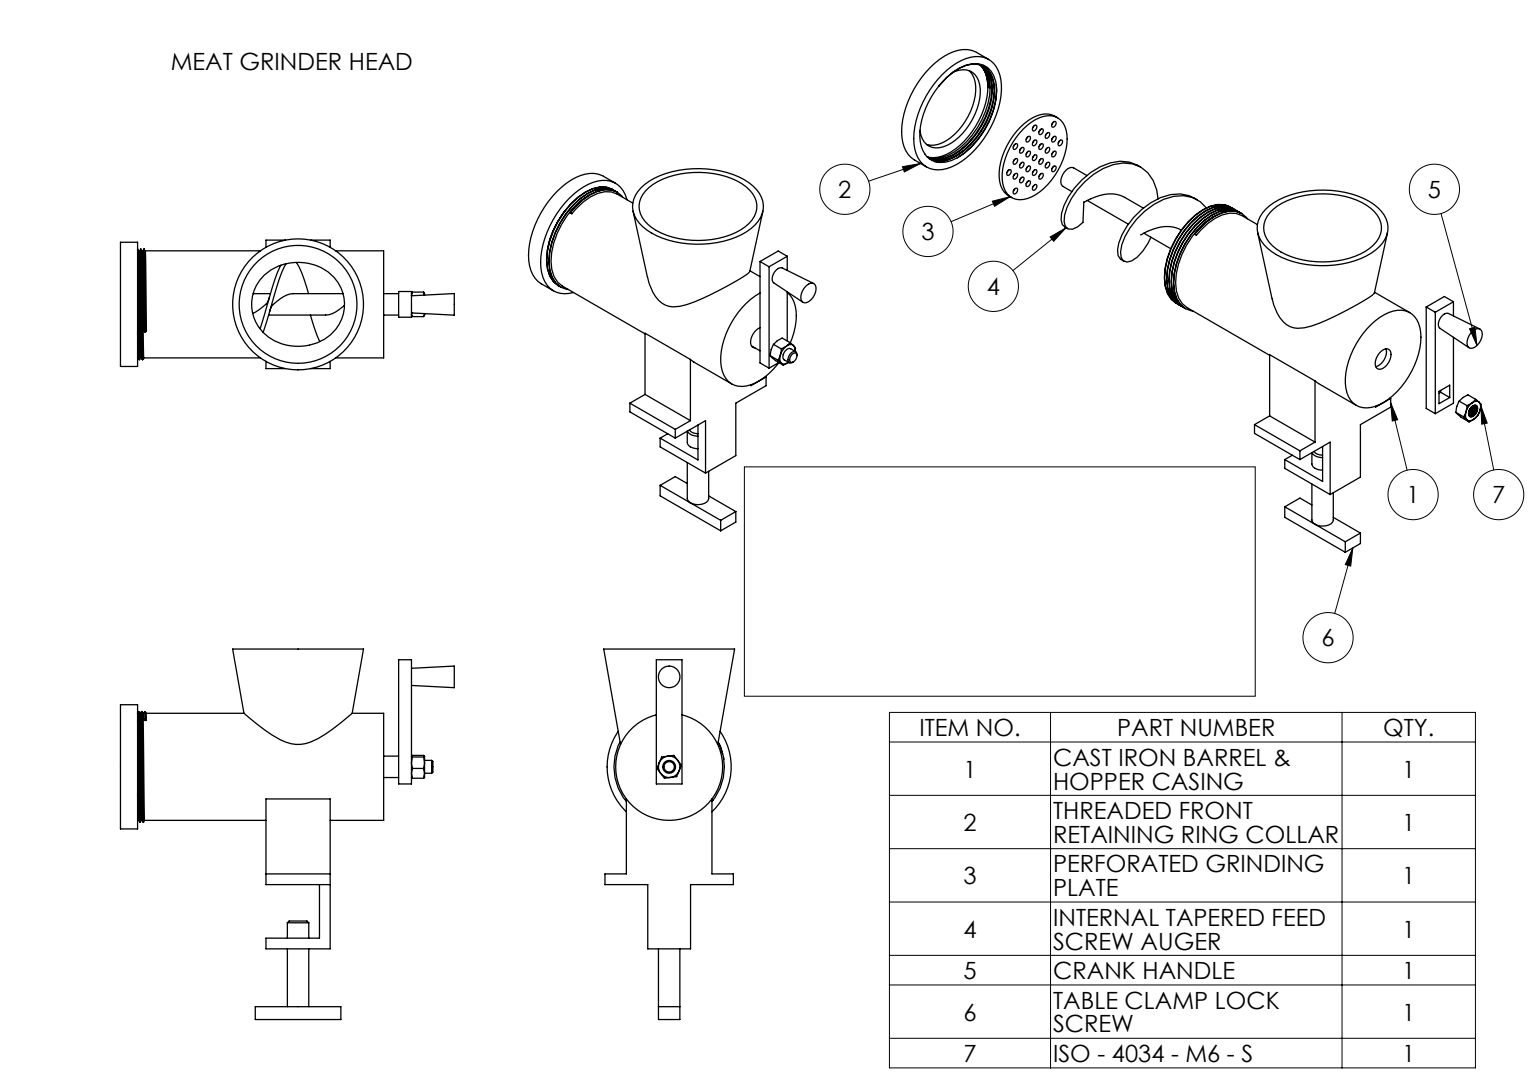
ISO-10303-21;
HEADER;
FILE_DESCRIPTION (('STEP AP214'),
    '1' );
FILE_NAME ('MAS-170',
    '2026-10-22T10:02:39',
    ( '' ),
    ( '' ),
    'SwSTEP 2.0',
    'SolidWorks 2026',
    '' );
FILE_SCHEMA (( 'AUTOMOTIVE_DESIGN' ));
ENDSEC;

DATA;
#1 = CARTESIAN_POINT ( 'NONE',  ( -15.00000000000000000, 55.00000000000000000, -20.00000000000000000 ) ) ;
#2 = AXIS2_PLACEMENT_3D ( 'NONE', #2206, #5818, #4912 ) ;
#3 = CARTESIAN_POINT ( 'NONE',  ( -24.57385867913225042, 55.01967498809302981, -0.01734603766092172178 ) ) ;
#4 = APPLICATION_PROTOCOL_DEFINITION ( 'draft international standard', 'automotive_design', 1998, #10813 ) ;
#5 = CARTESIAN_POINT ( 'NONE',  ( -21.63041020058595976, 76.92929161012460781, 1.799941901431467484 ) ) ;
#6 = VECTOR ( 'NONE', #483, 1000.000000000000000 ) ;
#7 = CIRCLE ( 'NONE', #1554, 1.500000000000001332 ) ;
#8 = CARTESIAN_POINT ( 'NONE',  ( -15.84874342590320673, 58.76832510134365606, 3.302529147201385129 ) ) ;
#9 = ORIENTED_EDGE ( 'NONE', *, *, #6036, .T. ) ;
#10 = CARTESIAN_POINT ( 'NONE',  ( -15.00000000000000000, 5.000000000000000000, 20.00000000000000000 ) ) ;
#11 = VERTEX_POINT ( 'NONE', #2092 ) ;
#12 = CARTESIAN_POINT ( 'NONE',  ( 7.477680471578420196, 36.66673471410030061, 10.56605622896702990 ) ) ;
#13 = CARTESIAN_POINT ( 'NONE',  ( -73.34375000204839523, 73.25176868561975141, -18.25176868561974430 ) ) ;
#14 = AXIS2_PLACEMENT_3D ( 'NONE', #9720, #5068, #10559 ) ;
#15 = EDGE_LOOP ( 'NONE', ( #10379, #7375, #3120, #371 ) ) ;
#16 = CARTESIAN_POINT ( 'NONE',  ( -75.12500000204838102, 44.30836144126050158, -25.81189881249999374 ) ) ;
#17 = CARTESIAN_POINT ( 'NONE',  ( 3.697305843545918513, 35.98616635274733255, -8.992456113074794644 ) ) ;
#18 = EDGE_CURVE ( 'NONE', #2366, #7152, #6007, .T. ) ;
#19 = VERTEX_POINT ( 'NONE', #7735 ) ;
#20 = APPLICATION_CONTEXT ( 'automotive_design' ) ;
#21 = CARTESIAN_POINT ( 'NONE',  ( -78.00000000000001421, 59.24264068711927678, 4.242644059037073312 ) ) ;
#22 = CARTESIAN_POINT ( 'NONE',  ( 18.90732451447525975, 55.01449046109523522, 0.007799356525960917524 ) ) ;
#23 = ORIENTED_EDGE ( 'NONE', *, *, #2675, .T. ) ;
#24 = CARTESIAN_POINT ( 'NONE',  ( -46.47759630686348942, 71.80626330759284315, -12.92347896748408509 ) ) ;
#25 = CARTESIAN_POINT ( 'NONE',  ( -13.52239577877046095, 75.98118489547775312, -2.745668029642679642 ) ) ;
#26 = CARTESIAN_POINT ( 'NONE',  ( 0.000000000000000000, 5.773502691896260863, -5.653418012614792154 ) ) ;
#27 = DIRECTION ( 'NONE',  ( 0.000000000000000000, 0.000000000000000000, 1.000000000000000000 ) ) ;
#28 = CARTESIAN_POINT ( 'NONE',  ( -78.00000000000001421, 50.75735931288069480, -11.22791868944003824 ) ) ;
#29 = DIRECTION ( 'NONE',  ( -1.000000000000000000, -0.000000000000000000, -0.000000000000000000 ) ) ;
#30 = VERTEX_POINT ( 'NONE', #8511 ) ;
#31 = CARTESIAN_POINT ( 'NONE',  ( -76.62500000409677625, 55.00000000000000000, 24.99999999999999645 ) ) ;
#32 = CARTESIAN_POINT ( 'NONE',  ( -54.99787500575298083, 55.00175321043320764, 0.0009066026748406779724 ) ) ;
#33 = CARTESIAN_POINT ( 'NONE',  ( -34.13164850161200548, 51.02358645912743640, -3.048757558511538068 ) ) ;
#34 = CARTESIAN_POINT ( 'NONE',  ( -80.00000000000001421, 63.48528137423857487, 8.485284746156350977 ) ) ;
#35 = EDGE_CURVE ( 'NONE', #6873, #1790, #10415, .T. ) ;
#36 = DIRECTION ( 'NONE',  ( 0.000000000000000000, 1.000000000000000000, 0.000000000000000000 ) ) ;
#37 = ORIENTED_EDGE ( 'NONE', *, *, #7774, .F. ) ;
#38 = CARTESIAN_POINT ( 'NONE',  ( -1.477628194636992243, 49.49121550494065502, -20.47411891050684218 ) ) ;
#39 = LINE ( 'NONE', #6477, #6145 ) ;
#40 = CARTESIAN_POINT ( 'NONE',  ( 10.96071222073927132, 53.39157304099641266, 4.745597011473480009 ) ) ;
#41 = CARTESIAN_POINT ( 'NONE',  ( -74.00000000204839523, 29.18810118750000981, 10.69163855873950020 ) ) ;
#42 = CARTESIAN_POINT ( 'NONE',  ( -78.87500000204838102, 65.69163855873949842, 25.81189881250000440 ) ) ;
#43 = VERTEX_POINT ( 'NONE', #10470 ) ;
#44 = CARTESIAN_POINT ( 'NONE',  ( -76.71875000204839523, 29.18810118750000271, 4.741568889096522788E-15 ) ) ;
#45 = ORIENTED_EDGE ( 'NONE', *, *, #4555, .T. ) ;
#46 = CARTESIAN_POINT ( 'NONE',  ( 3.204603673684104592, 51.02314964536983410, -3.048084100943247332 ) ) ;
#47 = CARTESIAN_POINT ( 'NONE',  ( -28.33520174651890144, 42.04728119469179148, 5.364820852706460030 ) ) ;
#48 = EDGE_CURVE ( 'NONE', #8851, #443, #4129, .T. ) ;
#49 = DIRECTION ( 'NONE',  ( 1.000000000000000000, 0.000000000000000000, 0.000000000000000000 ) ) ;
#50 = LINE ( 'NONE', #11190, #9309 ) ;
#51 = CARTESIAN_POINT ( 'NONE',  ( -78.03125000000002842, 79.99999999999992895, 10.35533905932734378 ) ) ;
#52 = VERTEX_POINT ( 'NONE', #2215 ) ;
#53 = CARTESIAN_POINT ( 'NONE',  ( -79.25000000000000000, 55.00000000000000000, 24.99999999999999645 ) ) ;
#54 = CARTESIAN_POINT ( 'NONE',  ( -72.59375000204838102, 55.00000000000000000, 25.81189881249999729 ) ) ;
#55 = EDGE_CURVE ( 'NONE', #2377, #9420, #11722, .T. ) ;
#56 = CARTESIAN_POINT ( 'NONE',  ( 0.000000000000000000, 0.000000000000000000, -6.099999999999999645 ) ) ;
#57 = B_SPLINE_CURVE_WITH_KNOTS ( 'NONE', 3,
 ( #11398, #9893, #5467, #4168 ),
 .UNSPECIFIED., .F., .F.,
 ( 4, 4 ),
 ( 2.380735200816727406E-07, 0.002921158011986720298 ),
 .UNSPECIFIED. ) ;
#58 = VECTOR ( 'NONE', #4245, 1000.000000000000000 ) ;
#59 = CARTESIAN_POINT ( 'NONE',  ( -47.09272475956910142, 55.02483394329467359, -0.008490977716145282211 ) ) ;
#60 = SHAPE_DEFINITION_REPRESENTATION ( #9305, #2176 ) ;
#61 = ADVANCED_FACE ( 'NONE', ( #1382, #293, #5043, #8690, #5765, #7618, #472, #11246, #4861, #6728, #10360, #351, #7675, #5881, #9524, #9811, #11776, #5272, #7139, #8090, #4373, #7912, #9698, #7079, #1495, #5216, #7192, #9040, #7965, #8982 ), #11541, .F. ) ;
#62 = CARTESIAN_POINT ( 'NONE',  ( -19.12261397941723473, 74.85860496676178855, 9.489298872914485372 ) ) ;
#63 = ADVANCED_FACE ( 'NONE', ( #6296 ), #11663, .F. ) ;
#64 = EDGE_CURVE ( 'NONE', #4200, #8679, #1605, .T. ) ;
#65 = DIRECTION ( 'NONE',  ( -0.000000000000000000, -1.000000000000000000, -0.000000000000000000 ) ) ;
#66 = VERTEX_POINT ( 'NONE', #6237 ) ;
#67 = DIRECTION ( 'NONE',  ( -1.000000000000000000, 0.000000000000000000, 0.000000000000000000 ) ) ;
#68 = FACE_OUTER_BOUND ( 'NONE', #814, .T. ) ;
#69 = VERTEX_POINT ( 'NONE', #11601 ) ;
#70 = CARTESIAN_POINT ( 'NONE',  ( -62.96917444215183224, 46.00616310598284286, 19.01165851688606523 ) ) ;
#71 = CARTESIAN_POINT ( 'NONE',  ( -71.59560441781462714, 80.81189881250000440, 6.916273779317701376 ) ) ;
#72 = EDGE_CURVE ( 'NONE', #8769, #5516, #701, .T. ) ;
#73 = ADVANCED_FACE ( 'NONE', ( #817 ), #4433, .F. ) ;
#74 = ORIENTED_EDGE ( 'NONE', *, *, #10875, .F. ) ;
#75 = EDGE_CURVE ( 'NONE', #3733, #9858, #3524, .T. ) ;
#76 = CARTESIAN_POINT ( 'NONE',  ( -72.50000000204839523, 29.18810118750000981, 10.69163855873950020 ) ) ;
#77 = CARTESIAN_POINT ( 'NONE',  ( -27.49360061100878738, 37.45598436699922473, 11.71495266747331421 ) ) ;
#78 = DIRECTION ( 'NONE',  ( -1.000000000000000000, 0.000000000000000000, 0.000000000000000000 ) ) ;
#79 = EDGE_LOOP ( 'NONE', ( #6944, #10404, #6581, #2124 ) ) ;
#80 = CARTESIAN_POINT ( 'NONE',  ( -12.37832547621337476, 59.49517489534859749, -2.213937092042313814 ) ) ;
#81 = COLOUR_RGB ( '',0.8941176470588234615, 0.8941176470588234615, 0.8941176470588234615 ) ;
#82 = CARTESIAN_POINT ( 'NONE',  ( -3.477628190354089099, 49.49309465598528845, -20.46958112014059950 ) ) ;
#83 = ORIENTED_EDGE ( 'NONE', *, *, #6664, .F. ) ;
#84 = CARTESIAN_POINT ( 'NONE',  ( -23.14426256960421924, 52.25445662165124361, 21.02210202263520600 ) ) ;
#85 = CARTESIAN_POINT ( 'NONE',  ( -68.81799204399976588, 34.52608862562686909, 5.501299279293338174 ) ) ;
#86 = LINE ( 'NONE', #1108, #4140 ) ;
#87 = DIRECTION ( 'NONE',  ( 1.000000000000000000, 0.000000000000000000, 0.000000000000000000 ) ) ;
#88 = LINE ( 'NONE', #7135, #10139 ) ;
#89 = VERTEX_POINT ( 'NONE', #9752 ) ;
#90 = CARTESIAN_POINT ( 'NONE',  ( -78.00000000000002842, 54.99999999999998579, 15.47056612039490986 ) ) ;
#91 = CARTESIAN_POINT ( 'NONE',  ( -44.20488284339200646, 55.00025175640378450, -0.002624240123811788852 ) ) ;
#92 = CARTESIAN_POINT ( 'NONE',  ( -56.68145153021548310, 56.29769244905448744, 4.839614506206188160 ) ) ;
#93 = CARTESIAN_POINT ( 'NONE',  ( 9.999999999999994671, -24.99999999999999645, 10.00000000000000000 ) ) ;
#94 = CARTESIAN_POINT ( 'NONE',  ( 47.00000000000000000, 55.00000000000000000, 0.000000000000000000 ) ) ;
#95 = CARTESIAN_POINT ( 'NONE',  ( -6.249156589778054105, 55.68730665650835476, -7.012895309292545676 ) ) ;
#96 = VERTEX_POINT ( 'NONE', #6118 ) ;
#97 = DIRECTION ( 'NONE',  ( 0.000000000000000000, -0.000000000000000000, 1.000000000000000000 ) ) ;
#98 = CARTESIAN_POINT ( 'NONE',  ( -71.75000000204838102, 80.81189881250000440, -10.69163855873948954 ) ) ;
#99 = CARTESIAN_POINT ( 'NONE',  ( 3.371861548457865722E-15, 110.0000000000000000, -27.53333900685068869 ) ) ;
#100 = CARTESIAN_POINT ( 'NONE',  ( -3.000000000000000000, 0.000000000000000000, -1.753742857142857048 ) ) ;
#101 = CARTESIAN_POINT ( 'NONE',  ( 0.000000000000000000, -24.99999999999999645, -5.000000000000000000 ) ) ;
#102 = CARTESIAN_POINT ( 'NONE',  ( -80.00000000000002842, 38.02943725152282184, 3.371917797929946392E-06 ) ) ;
#103 = AXIS2_PLACEMENT_3D ( 'NONE', #3802, #8297, #78 ) ;
#104 = ORIENTED_EDGE ( 'NONE', *, *, #11406, .F. ) ;
#105 = CARTESIAN_POINT ( 'NONE',  ( -77.65625000204839523, 73.25176868561975141, -18.25176868561974430 ) ) ;
#106 = ORIENTED_EDGE ( 'NONE', *, *, #10406, .T. ) ;
#107 = CARTESIAN_POINT ( 'NONE',  ( 24.10175047695886619, 78.98596163070220655, -7.059706225875322261 ) ) ;
#108 = CARTESIAN_POINT ( 'NONE',  ( -34.53957387867419015, 43.82314937793580611, -8.587433708483555250 ) ) ;
#109 = VECTOR ( 'NONE', #311, 1000.000000000000000 ) ;
#110 = CARTESIAN_POINT ( 'NONE',  ( -77.75000000204839523, 65.69163855873948421, -25.81189881250000084 ) ) ;
#111 = EDGE_CURVE ( 'NONE', #9073, #8979, #3345, .T. ) ;
#112 = DIRECTION ( 'NONE',  ( 0.000000000000000000, -0.000000000000000000, 1.000000000000000000 ) ) ;
#113 = DIRECTION ( 'NONE',  ( 0.000000000000000000, 0.000000000000000000, 1.000000000000000000 ) ) ;
#114 = ORIENTED_EDGE ( 'NONE', *, *, #10655, .T. ) ;
#115 = VECTOR ( 'NONE', #7085, 1000.000000000000000 ) ;
#116 = CARTESIAN_POINT ( 'NONE',  ( -78.31250000000000000, 72.67766952966368876, -17.67766952966368876 ) ) ;
#117 = CARTESIAN_POINT ( 'NONE',  ( -78.50000000409677625, 80.00000000000000000, -1.530808498934191324E-15 ) ) ;
#118 = CIRCLE ( 'NONE', #8173, 1.500000000000001332 ) ;
#119 = CARTESIAN_POINT ( 'NONE',  ( -78.00000000000001421, 50.75735931288069480, -12.72791868944003824 ) ) ;
#120 = DIRECTION ( 'NONE',  ( 1.000000000000000000, 0.000000000000000000, -0.000000000000000000 ) ) ;
#121 = CARTESIAN_POINT ( 'NONE',  ( -53.33538954556567546, 54.99810722428492937, -0.002143453996954131253 ) ) ;
#122 = SHAPE_DEFINITION_REPRESENTATION ( #1837, #423 ) ;
#123 = B_SPLINE_CURVE_WITH_KNOTS ( 'NONE', 3,
 ( #9839, #9954, #7047, #10669, #4339, #2656 ),
 .UNSPECIFIED., .F., .F.,
 ( 4, 2, 4 ),
 ( 0.008070708573309213693, 0.009531758523483282314, 0.01099280847365734920 ),
 .UNSPECIFIED. ) ;
#124 = CARTESIAN_POINT ( 'NONE',  ( -10.64432325360710152, 68.67941443230903076, -17.23560473394323367 ) ) ;
#125 = AXIS2_PLACEMENT_3D ( 'NONE', #5377, #67, #9915 ) ;
#126 = CARTESIAN_POINT ( 'NONE',  ( -5.000000000000000000, 0.000000000000000000, -6.099999999999999645 ) ) ;
#127 = AXIS2_PLACEMENT_3D ( 'NONE', #5632, #97, #11119 ) ;
#128 = ORIENTED_EDGE ( 'NONE', *, *, #8290, .T. ) ;
#129 = CARTESIAN_POINT ( 'NONE',  ( -79.34375000000000000, 65.35533905932734910, 24.99999999999997158 ) ) ;
#130 = CYLINDRICAL_SURFACE ( 'NONE', #5375, 1.500000000000000000 ) ;
#131 = VERTEX_POINT ( 'NONE', #8809 ) ;
#132 = CARTESIAN_POINT ( 'NONE',  ( -6.160267096003628318, 59.12214581854949103, -20.69010011304746044 ) ) ;
#133 = PRODUCT_DEFINITION ( 'UNKNOWN', '', #852, #2465 ) ;
#134 = CARTESIAN_POINT ( 'NONE',  ( -76.71875000204839523, 29.18810118750000271, 4.741568889096522788E-15 ) ) ;
#135 = CARTESIAN_POINT ( 'NONE',  ( -15.00000000000000355, 5.000000000000000000, -29.99999999999999289 ) ) ;
#136 = CARTESIAN_POINT ( 'NONE',  ( -6.214759040711413718, 65.81103152010582846, -18.03762937187994453 ) ) ;
#137 = CARTESIAN_POINT ( 'NONE',  ( -46.52239103091250172, 73.32882989972571863, -10.56393531560676102 ) ) ;
#138 = ORIENTED_EDGE ( 'NONE', *, *, #9495, .F. ) ;
#139 = LINE ( 'NONE', #1945, #11400 ) ;
#140 = EDGE_CURVE ( 'NONE', #7402, #8679, #2318, .T. ) ;
#141 = CARTESIAN_POINT ( 'NONE',  ( 46.99999999999999289, 58.53553390593273065, 3.535533905932731091 ) ) ;
#142 = CARTESIAN_POINT ( 'NONE',  ( 4.636023424558444184, 34.00634798409771520, 1.031279783234476222 ) ) ;
#143 = VECTOR ( 'NONE', #3904, 1000.000000000000000 ) ;
#144 = ORIENTED_EDGE ( 'NONE', *, *, #11561, .T. ) ;
#145 = CARTESIAN_POINT ( 'NONE',  ( -34.81092923608149192, 36.62878417468885317, -10.58136149031614970 ) ) ;
#146 = CARTESIAN_POINT ( 'NONE',  ( -70.34104699118840642, 33.99562393659799397, 0.006612473344882377653 ) ) ;
#147 = CARTESIAN_POINT ( 'NONE',  ( -73.34375000409679046, 30.00000000000001421, 10.35533905932739174 ) ) ;
#148 = DIRECTION ( 'NONE',  ( -1.000000000000000000, -0.000000000000000000, -0.000000000000000000 ) ) ;
#149 = EDGE_CURVE ( 'NONE', #1776, #658, #10646, .T. ) ;
#150 = CYLINDRICAL_SURFACE ( 'NONE', #7865, 1.499999999999999556 ) ;
#151 = EDGE_CURVE ( 'NONE', #658, #760, #3805, .T. ) ;
#152 = ORIENTED_EDGE ( 'NONE', *, *, #4340, .T. ) ;
#153 = DIRECTION ( 'NONE',  ( 0.000000000000000000, -0.000000000000000000, 1.000000000000000000 ) ) ;
#154 = CARTESIAN_POINT ( 'NONE',  ( -35.76380172564871884, 55.01086174631173975, 0.005834152228799136322 ) ) ;
#155 = CARTESIAN_POINT ( 'NONE',  ( -44.62221111874860213, 58.76649436596603948, -3.304682393689729381 ) ) ;
#156 = DIRECTION ( 'NONE',  ( -0.000000000000000000, -1.000000000000000000, -0.000000000000000000 ) ) ;
#157 = FACE_OUTER_BOUND ( 'NONE', #10390, .T. ) ;
#158 = CARTESIAN_POINT ( 'NONE',  ( -6.833556764572190190, 56.37289815856257746, -6.894355924324841567 ) ) ;
#159 = AXIS2_PLACEMENT_3D ( 'NONE', #745, #8186, #2789 ) ;
#160 = ORIENTED_EDGE ( 'NONE', *, *, #1242, .F. ) ;
#161 = CARTESIAN_POINT ( 'NONE',  ( 9.477680475861957277, 36.67126955513442255, 10.56417786655960356 ) ) ;
#162 = CARTESIAN_POINT ( 'NONE',  ( 0.000000000000000000, 0.000000000000000000, -0.01270000000000047133 ) ) ;
#163 = LINE ( 'NONE', #11122, #11282 ) ;
#164 = FACE_BOUND ( 'NONE', #3650, .T. ) ;
#165 = CARTESIAN_POINT ( 'NONE',  ( -12.37866201454132487, 69.98577131611273217, -20.01755997183146718 ) ) ;
#166 = CARTESIAN_POINT ( 'NONE',  ( -74.56250000204839523, 80.81189881250001861, 10.69163855873948599 ) ) ;
#167 = ORIENTED_EDGE ( 'NONE', *, *, #2613, .F. ) ;
#168 = CARTESIAN_POINT ( 'NONE',  ( -78.59375000204839523, 55.00000000000000000, 25.81189881249999729 ) ) ;
#169 = CIRCLE ( 'NONE', #3240, 1.500000000000001332 ) ;
#170 = ORIENTED_EDGE ( 'NONE', *, *, #3166, .T. ) ;
#171 = CARTESIAN_POINT ( 'NONE',  ( 3.392634454741613848, 65.79950035100726780, -22.54765914078175015 ) ) ;
#172 = AXIS2_PLACEMENT_3D ( 'NONE', #8865, #9866, #7078 ) ;
#173 = CARTESIAN_POINT ( 'NONE',  ( -30.96365390035560239, 40.99197526476194042, -0.6880654886566857087 ) ) ;
#174 = FACE_OUTER_BOUND ( 'NONE', #11292, .T. ) ;
#175 = ADVANCED_FACE ( 'NONE', ( #10161 ), #9210, .T. ) ;
#176 =( BOUNDED_CURVE ( )  B_SPLINE_CURVE ( 2, ( #5683, #4899, #11229, #6928, #8370, #6645, #9381, #4776, #5808 ),
 .UNSPECIFIED., .F., .T. ) 
 B_SPLINE_CURVE_WITH_KNOTS ( ( 3, 2, 2, 2, 3 ),
 ( 0.3333333333333335924, 0.3541666666666669627, 0.3750000000000003331, 0.3958333333333336479, 0.4166666666666670182 ),
 .UNSPECIFIED. ) 
 CURVE ( )  GEOMETRIC_REPRESENTATION_ITEM ( )  RATIONAL_B_SPLINE_CURVE ( ( 0.9999999999999990008, 0.9238795325112877377, 1.000000000000000000, 0.9238795325112867385, 1.000000000000000000, 0.9238795325112867385, 1.000000000000000000, 0.9238795325112855172, 1.000000000000001110 ) ) 
 REPRESENTATION_ITEM ( '' )  );
#177 = CARTESIAN_POINT ( 'NONE',  ( -75.00000000000000000, 63.49954157109033304, -24.30489545910771909 ) ) ;
#178 = CARTESIAN_POINT ( 'NONE',  ( -15.00000000000000355, 0.000000000000000000, -29.99999999999999289 ) ) ;
#179 = VECTOR ( 'NONE', #1295, 1000.000000000000000 ) ;
#180 = CIRCLE ( 'NONE', #6902, 2.500000000000000000 ) ;
#181 = EDGE_LOOP ( 'NONE', ( #6646, #3991, #9037, #3173 ) ) ;
#182 = FACE_OUTER_BOUND ( 'NONE', #3755, .T. ) ;
#183 = CYLINDRICAL_SURFACE ( 'NONE', #11845, 1.500000000000000444 ) ;
#184 = DIRECTION ( 'NONE',  ( 0.000000000000000000, 0.000000000000000000, 1.000000000000000000 ) ) ;
#185 = CARTESIAN_POINT ( 'NONE',  ( 0.000000000000000000, 0.000000000000000000, -2.617914285714285416 ) ) ;
#186 = CARTESIAN_POINT ( 'NONE',  ( 6.125158419864718873, 48.06305152834397632, -1.028633690847041704 ) ) ;
#187 = CARTESIAN_POINT ( 'NONE',  ( -7.638500494831339971, 67.00046308197731548, 18.44294210305378456 ) ) ;
#188 = DIRECTION ( 'NONE',  ( 0.000000000000000000, 0.000000000000000000, 1.000000000000000000 ) ) ;
#189 = EDGE_LOOP ( 'NONE', ( #2988, #1101, #3191 ) ) ;
#190 = EDGE_CURVE ( 'NONE', #2213, #10233, #9603, .T. ) ;
#191 = FACE_OUTER_BOUND ( 'NONE', #2836, .T. ) ;
#192 = DIRECTION ( 'NONE',  ( 0.000000000000000000, 0.000000000000000000, 1.000000000000000000 ) ) ;
#193 = VERTEX_POINT ( 'NONE', #2983 ) ;
#194 = CARTESIAN_POINT ( 'NONE',  ( -66.50782127702024127, 36.67013743889115318, 10.55179617378401247 ) ) ;
#195 = VECTOR ( 'NONE', #5572, 1000.000000000000000 ) ;
#196 = CARTESIAN_POINT ( 'NONE',  ( -78.68750000204839523, 65.69163855873949842, 25.81189881250000440 ) ) ;
#197 = EDGE_CURVE ( 'NONE', #1911, #3047, #4966, .T. ) ;
#198 = DIRECTION ( 'NONE',  ( 6.033820786006286457E-17, -1.000000000000000000, 0.000000000000000000 ) ) ;
#199 = CARTESIAN_POINT ( 'NONE',  ( -42.66281101964754896, 63.04450918361814615, -19.42252581123130639 ) ) ;
#200 = AXIS2_PLACEMENT_3D ( 'NONE', #7923, #603, #5167 ) ;
#201 = CONICAL_SURFACE ( 'NONE', #2897, 2.500000000000000000, 0.9599310885968755924 ) ;
#202 = PRESENTATION_STYLE_ASSIGNMENT (( #2843 ) ) ;
#203 = CARTESIAN_POINT ( 'NONE',  ( -30.99614452189004155, 33.97742542711323921, 0.0005215828242728561687 ) ) ;
#204 = ORIENTED_EDGE ( 'NONE', *, *, #9495, .T. ) ;
#205 = CARTESIAN_POINT ( 'NONE',  ( -71.93750000204838102, 44.30836144126049447, -25.81189881249999019 ) ) ;
#206 = EDGE_CURVE ( 'NONE', #6519, #11654, #6983, .T. ) ;
#207 = DIRECTION ( 'NONE',  ( -1.000000000000000000, -0.000000000000000000, -0.000000000000000000 ) ) ;
#208 = FACE_OUTER_BOUND ( 'NONE', #5773, .T. ) ;
#209 = ORIENTED_EDGE ( 'NONE', *, *, #10668, .T. ) ;
#210 = CARTESIAN_POINT ( 'NONE',  ( -56.17294560383920299, 66.73154858138525469, 17.54339796666672058 ) ) ;
#211 = CIRCLE ( 'NONE', #6745, 2.500000000000000000 ) ;
#212 = CARTESIAN_POINT ( 'NONE',  ( -61.00490302436042356, 55.00059028654953153, 21.02810969917934614 ) ) ;
#213 = FILL_AREA_STYLE_COLOUR ( '', #499 ) ;
#214 = CARTESIAN_POINT ( 'NONE',  ( -75.87500000409677625, 55.00000000000000000, -24.99999999999999645 ) ) ;
#215 = VECTOR ( 'NONE', #1197, 1000.000000000000000 ) ;
#216 = CARTESIAN_POINT ( 'NONE',  ( 53.00000000000000000, 51.46446609406726935, -3.535533905932738197 ) ) ;
#217 = CARTESIAN_POINT ( 'NONE',  ( 47.00000000000000000, 55.00000000000000000, 6.000000000000000000 ) ) ;
#218 = ORIENTED_EDGE ( 'NONE', *, *, #5065, .F. ) ;
#219 = CARTESIAN_POINT ( 'NONE',  ( -78.31250000000000000, 72.67766952966368876, -17.67766952966368876 ) ) ;
#220 = CARTESIAN_POINT ( 'NONE',  ( -14.57393009465980604, 54.98364064865898371, -0.001646604999752838971 ) ) ;
#221 = DIRECTION ( 'NONE',  ( 0.5000000000000005551, -0.8660254037844383745, 0.000000000000000000 ) ) ;
#222 = AXIS2_PLACEMENT_3D ( 'NONE', #671, #2237, #9611 ) ;
#223 = DIRECTION ( 'NONE',  ( -1.000000000000000000, -6.033820786006286457E-17, 0.000000000000000000 ) ) ;
#224 = CARTESIAN_POINT ( 'NONE',  ( 0.1668379413723253268, 49.14794564670181387, -3.906842406148068214 ) ) ;
#225 = ORIENTED_EDGE ( 'NONE', *, *, #438, .T. ) ;
#226 = CARTESIAN_POINT ( 'NONE',  ( 14.14423903981857755, 49.50929293985068114, 20.43023407247793699 ) ) ;
#227 = DIRECTION ( 'NONE',  ( 0.000000000000000000, 0.000000000000000000, 1.000000000000000000 ) ) ;
#228 = PLANE ( 'NONE',  #2565 ) ;
#229 = CARTESIAN_POINT ( 'NONE',  ( 73.00000000000000000, 91.95184441433917755, -3.614966813601447167E-16 ) ) ;
#230 = CARTESIAN_POINT ( 'NONE',  ( -71.84375000204838102, 73.25176868561975141, -18.25176868561974430 ) ) ;
#231 = CARTESIAN_POINT ( 'NONE',  ( -71.59560441781462714, 80.81189881250000440, 6.916273779317701376 ) ) ;
#232 = ORIENTED_EDGE ( 'NONE', *, *, #8402, .T. ) ;
#233 = CARTESIAN_POINT ( 'NONE',  ( -76.06250000409679046, 37.32233047033631124, -17.67766952966368166 ) ) ;
#234 = ORIENTED_EDGE ( 'NONE', *, *, #5652, .T. ) ;
#235 = CARTESIAN_POINT ( 'NONE',  ( 23.67201755683229081, 78.62200754200915753, -8.225812365109568702 ) ) ;
#236 = EDGE_CURVE ( 'NONE', #9206, #11519, #5249, .T. ) ;
#237 = CARTESIAN_POINT ( 'NONE',  ( -55.16972311799333539, 62.82217562642412645, 11.69677751401117405 ) ) ;
#238 = CARTESIAN_POINT ( 'NONE',  ( -78.87500000204839523, 65.69163855873949842, 25.81189881250000084 ) ) ;
#239 = CARTESIAN_POINT ( 'NONE',  ( -75.00000000000002842, 78.51577914341699227, 8.706246595591601078 ) ) ;
#240 = CARTESIAN_POINT ( 'NONE',  ( -2.500000000000000000, 3.061616997868383141E-16, -6.099999999999999645 ) ) ;
#241 = VERTEX_POINT ( 'NONE', #2085 ) ;
#242 = DIRECTION ( 'NONE',  ( 0.000000000000000000, -0.000000000000000000, 1.000000000000000000 ) ) ;
#243 = FACE_OUTER_BOUND ( 'NONE', #10356, .T. ) ;
#244 = LINE ( 'NONE', #4871, #4047 ) ;
#245 = FACE_BOUND ( 'NONE', #9079, .T. ) ;
#246 = CARTESIAN_POINT ( 'NONE',  ( -18.95794697780666027, 57.36371471763808927, 6.606639808170175598 ) ) ;
#247 = DIRECTION ( 'NONE',  ( -1.000000000000000000, -0.000000000000000000, -0.000000000000000000 ) ) ;
#248 = DIRECTION ( 'NONE',  ( -1.000000000000000000, -0.000000000000000000, -0.000000000000000000 ) ) ;
#249 = EDGE_LOOP ( 'NONE', ( #1338, #6982, #2879, #8696 ) ) ;
#250 = CARTESIAN_POINT ( 'NONE',  ( -78.00000000000002842, 42.27207793864211283, -4.242637315201479353 ) ) ;
#251 = CARTESIAN_POINT ( 'NONE',  ( 52.99999999999999289, 58.53553390593273065, 3.535533905932731091 ) ) ;
#252 = ORIENTED_EDGE ( 'NONE', *, *, #5075, .F. ) ;
#253 = CARTESIAN_POINT ( 'NONE',  ( -59.27472368810988002, 61.13901599248961105, 20.20251803659174783 ) ) ;
#254 = CARTESIAN_POINT ( 'NONE',  ( -75.87500000204839523, 80.81189881250001861, 10.69163855873948599 ) ) ;
#255 = DIRECTION ( 'NONE',  ( -1.000000000000000000, -0.000000000000000000, -0.000000000000000000 ) ) ;
#256 = CARTESIAN_POINT ( 'NONE',  ( -50.82691677660828589, 75.68920158268997511, 4.121780573430135597 ) ) ;
#257 =( NAMED_UNIT ( * ) SI_UNIT ( $, .STERADIAN. ) SOLID_ANGLE_UNIT ( ) );
#258 = DIRECTION ( 'NONE',  ( 0.000000000000000000, 1.000000000000000000, 0.000000000000000000 ) ) ;
#259 = ORIENTED_EDGE ( 'NONE', *, *, #6814, .T. ) ;
#260 = CIRCLE ( 'NONE', #1600, 3.000000000000000888 ) ;
#261 = CARTESIAN_POINT ( 'NONE',  ( -73.71875000204839523, 29.18810118750000271, 4.741568889096522788E-15 ) ) ;
#262 = PLANE ( 'NONE',  #3428 ) ;
#263 = ADVANCED_FACE ( 'NONE', ( #10291 ), #10352, .F. ) ;
#264 = CARTESIAN_POINT ( 'NONE',  ( -3.000000000000000000, 0.000000000000000000, -5.210428571428570521 ) ) ;
#265 = ORIENTED_EDGE ( 'NONE', *, *, #8549, .F. ) ;
#266 = ADVANCED_FACE ( 'NONE', ( #3949 ), #228, .F. ) ;
#267 = CARTESIAN_POINT ( 'NONE',  ( -58.49417186384191325, 59.10997037288393585, 20.69225924102262226 ) ) ;
#268 = CARTESIAN_POINT ( 'NONE',  ( 14.87282114002693234, 58.67269055319452065, 13.65170787854068024 ) ) ;
#269 = CYLINDRICAL_SURFACE ( 'NONE', #2101, 1.499999999999999556 ) ;
#270 = CARTESIAN_POINT ( 'NONE',  ( -76.34375000409679046, 30.00000000000001421, 10.35533905932739174 ) ) ;
#271 = FACE_OUTER_BOUND ( 'NONE', #5676, .T. ) ;
#272 = CARTESIAN_POINT ( 'NONE',  ( -72.06435441788595142, 79.99999999999991473, 6.698726029249561620 ) ) ;
#273 = ADVANCED_FACE ( 'NONE', ( #4913 ), #344, .F. ) ;
#274 = ORIENTED_EDGE ( 'NONE', *, *, #7349, .T. ) ;
#275 = CARTESIAN_POINT ( 'NONE',  ( -79.53125000000000000, 80.00000000000001421, 10.35533905932737397 ) ) ;
#276 = CARTESIAN_POINT ( 'NONE',  ( -68.24753854205350478, 55.02494518472502705, -0.0008082322394851507684 ) ) ;
#277 = AXIS2_PLACEMENT_3D ( 'NONE', #2600, #1465, #2419 ) ;
#278 = PLANE ( 'NONE',  #4388 ) ;
#279 = CARTESIAN_POINT ( 'NONE',  ( -15.00000000000000000, -24.99999999999999645, 10.00000000000000000 ) ) ;
#280 = CARTESIAN_POINT ( 'NONE',  ( -69.87738456456679614, 41.01771127808763140, 1.829669757797043994 ) ) ;
#281 = ORIENTED_EDGE ( 'NONE', *, *, #2765, .F. ) ;
#282 = DIRECTION ( 'NONE',  ( -1.000000000000000000, -0.000000000000000000, -0.000000000000000000 ) ) ;
#283 = CARTESIAN_POINT ( 'NONE',  ( 36.99999999999999289, 59.99999999999998579, 0.000000000000000000 ) ) ;
#284 = CARTESIAN_POINT ( 'NONE',  ( 53.00000000000000000, 51.46446609406726935, -3.535533905932738197 ) ) ;
#285 = DIRECTION ( 'NONE',  ( -0.8191520442889885789, 1.003171929053520802E-16, 0.5735764363510507113 ) ) ;
#286 = PRODUCT_RELATED_PRODUCT_CATEGORY ( 'part', '', ( #7403 ) ) ;
#287 = DIRECTION ( 'NONE',  ( 0.000000000000000000, 0.000000000000000000, -1.000000000000000000 ) ) ;
#288 = CARTESIAN_POINT ( 'NONE',  ( -77.93750000204838102, 44.30836144126050158, -25.81189881249999374 ) ) ;
#289 = CIRCLE ( 'NONE', #9478, 3.000000000000000000 ) ;
#290 = ORIENTED_EDGE ( 'NONE', *, *, #8254, .T. ) ;
#291 = EDGE_CURVE ( 'NONE', #2366, #8948, #1373, .T. ) ;
#292 = CARTESIAN_POINT ( 'NONE',  ( -73.62500000204842365, 29.18810118750000626, -10.69163855873949309 ) ) ;
#293 = FACE_BOUND ( 'NONE', #10060, .T. ) ;
#294 = DIRECTION ( 'NONE',  ( -1.000000000000000000, 0.000000000000000000, -0.000000000000000000 ) ) ;
#295 = CARTESIAN_POINT ( 'NONE',  ( -53.99820501230367142, 64.90985867132549458, 9.909159326440711624 ) ) ;
#296 = CARTESIAN_POINT ( 'NONE',  ( 0.000000000000000000, 0.000000000000000000, 10.00000000000000000 ) ) ;
#297 = CARTESIAN_POINT ( 'NONE',  ( -75.00000000000000000, 78.71525423744449768, -9.017306879578036671 ) ) ;
#298 = EDGE_CURVE ( 'NONE', #1810, #1322, #2665, .T. ) ;
#299 = EDGE_CURVE ( 'NONE', #11481, #8007, #11177, .T. ) ;
#300 = CARTESIAN_POINT ( 'NONE',  ( -20.00000000000003197, -57.00000000000000000, 5.000000000000000000 ) ) ;
#301 = VERTEX_POINT ( 'NONE', #1190 ) ;
#302 = AXIS2_PLACEMENT_3D ( 'NONE', #9626, #1421, #6826 ) ;
#303 = CARTESIAN_POINT ( 'NONE',  ( -77.28124999999998579, 30.00000000000000355, -10.35533905932738108 ) ) ;
#304 = CARTESIAN_POINT ( 'NONE',  ( -72.21875000409676204, 65.35533905932737753, 24.99999999999999645 ) ) ;
#305 = CARTESIAN_POINT ( 'NONE',  ( -77.00000000000000000, 55.00000000000000000, -24.99999999999999645 ) ) ;
#306 = VERTEX_POINT ( 'NONE', #4010 ) ;
#307 = EDGE_CURVE ( 'NONE', #8475, #1715, #7669, .T. ) ;
#308 = CARTESIAN_POINT ( 'NONE',  ( -24.89001229408545512, 50.71618230245203307, 5.579812370254800591 ) ) ;
#309 = CARTESIAN_POINT ( 'NONE',  ( -2.905210441188253778, 65.30173033721455056, 19.43922460838591348 ) ) ;
#310 = VECTOR ( 'NONE', #7758, 1000.000000000000227 ) ;
#311 = DIRECTION ( 'NONE',  ( 1.000000000000000000, 0.000000000000000000, 0.000000000000000000 ) ) ;
#312 = ORIENTED_EDGE ( 'NONE', *, *, #8953, .F. ) ;
#313 = DIRECTION ( 'NONE',  ( 0.000000000000000000, 0.000000000000000000, -1.000000000000000000 ) ) ;
#314 = CIRCLE ( 'NONE', #4535, 1.500000000000001332 ) ;
#315 = ORIENTED_EDGE ( 'NONE', *, *, #10681, .F. ) ;
#316 = CARTESIAN_POINT ( 'NONE',  ( -63.32723919479404628, 46.95276866351182576, 19.42062151208882170 ) ) ;
#317 = CARTESIAN_POINT ( 'NONE',  ( -73.90625000204839523, 36.74823131438026280, 18.25176868561974786 ) ) ;
#318 = CARTESIAN_POINT ( 'NONE',  ( 0.000000000000000000, 0.000000000000000000, -6.099999999999999645 ) ) ;
#319 = CARTESIAN_POINT ( 'NONE',  ( -56.05785376386896246, 64.93131079446247611, 18.59685268580366468 ) ) ;
#320 = CIRCLE ( 'NONE', #10069, 1.500000000000001332 ) ;
#321 = CARTESIAN_POINT ( 'NONE',  ( -68.34104732181945963, 33.99448141944315438, 0.006743540747239065887 ) ) ;
#322 = VERTEX_POINT ( 'NONE', #10463 ) ;
#323 = DIRECTION ( 'NONE',  ( -0.5000000000000006661, 0.8660254037844383745, 0.000000000000000000 ) ) ;
#324 = DIRECTION ( 'NONE',  ( 9.813077866773612233E-16, -1.000000000000000000, 0.000000000000000000 ) ) ;
#325 = CARTESIAN_POINT ( 'NONE',  ( 15.18896243380506306, 60.50666922109576262, 20.46968130491651650 ) ) ;
#326 = EDGE_LOOP ( 'NONE', ( #6442, #4542, #10386, #11390 ) ) ;
#327 = CARTESIAN_POINT ( 'NONE',  ( -61.99390593487224521, 46.95297697149054272, 19.42004845484624909 ) ) ;
#328 = AXIS2_PLACEMENT_3D ( 'NONE', #6832, #8558, #9628 ) ;
#329 = CARTESIAN_POINT ( 'NONE',  ( -61.59556246352555320, 52.94114603458827872, 20.93095456750423722 ) ) ;
#330 = CARTESIAN_POINT ( 'NONE',  ( -78.00000000000002842, 42.27207793864211283, -5.742637315201479353 ) ) ;
#331 = CONICAL_SURFACE ( 'NONE', #1858, 3.000000000000000000, 0.9599310885968912466 ) ;
#332 = DIRECTION ( 'NONE',  ( 0.000000000000000000, 0.000000000000000000, 1.000000000000000000 ) ) ;
#333 = CARTESIAN_POINT ( 'NONE',  ( -72.31250000000007105, 72.67766952966360350, -17.67766952966359995 ) ) ;
#334 = EDGE_LOOP ( 'NONE', ( #4076, #9464, #9647, #1105 ) ) ;
#335 = CARTESIAN_POINT ( 'NONE',  ( -75.96875000000000000, 30.00000000000001421, 10.35533905932739174 ) ) ;
#336 = CARTESIAN_POINT ( 'NONE',  ( -70.57370072173033293, 55.01541170666005343, -0.006042036165150080004 ) ) ;
#337 = FILL_AREA_STYLE_COLOUR ( '', #5158 ) ;
#338 = CIRCLE ( 'NONE', #8388, 3.000000000000000000 ) ;
#339 = DIRECTION ( 'NONE',  ( 0.000000000000000000, 0.000000000000000000, 1.000000000000000000 ) ) ;
#340 = CARTESIAN_POINT ( 'NONE',  ( 2.791825101730443404, 48.06463389261614338, -1.028630067443766283 ) ) ;
#341 = ORIENTED_EDGE ( 'NONE', *, *, #3274, .F. ) ;
#342 = CARTESIAN_POINT ( 'NONE',  ( -28.67054321954914542, 35.57240153874681710, 8.046710727719679213 ) ) ;
#343 = DIRECTION ( 'NONE',  ( 0.000000000000000000, 1.000000000000000000, 0.000000000000000000 ) ) ;
#344 = CYLINDRICAL_SURFACE ( 'NONE', #9643, 3.000000000000000888 ) ;
#345 = CARTESIAN_POINT ( 'NONE',  ( -78.00000000000001421, 50.75735931288069480, -4.242637315201482906 ) ) ;
#346 = CARTESIAN_POINT ( 'NONE',  ( -3.398726575883826762, 65.81855960629934543, 22.53824819929336698 ) ) ;
#347 = CARTESIAN_POINT ( 'NONE',  ( -76.81250000204839523, 29.18810118750000981, 10.69163855873950020 ) ) ;
#348 = EDGE_LOOP ( 'NONE', ( #11086, #2027, #10257, #10094 ) ) ;
#349 = EDGE_CURVE ( 'NONE', #1114, #2366, #8625, .T. ) ;
#350 = CARTESIAN_POINT ( 'NONE',  ( -78.21875000409679046, 65.35533905932737753, 24.99999999999999645 ) ) ;
#351 = FACE_BOUND ( 'NONE', #8937, .T. ) ;
#352 = CARTESIAN_POINT ( 'NONE',  ( 12.39308895597016047, 69.98013642987091032, -20.04675360703169318 ) ) ;
#353 = CARTESIAN_POINT ( 'NONE',  ( -58.37019661190561948, 55.68797971655733647, 13.99244826128962593 ) ) ;
#354 = FACE_BOUND ( 'NONE', #1822, .T. ) ;
#355 = AXIS2_PLACEMENT_3D ( 'NONE', #11527, #8791, #3333 ) ;
#356 = CARTESIAN_POINT ( 'NONE',  ( -80.00000000000002842, 42.27207793864211283, -2.742637315201478909 ) ) ;
#357 = FACE_OUTER_BOUND ( 'NONE', #4501, .T. ) ;
#358 = ORIENTED_EDGE ( 'NONE', *, *, #7637, .F. ) ;
#359 = VECTOR ( 'NONE', #9412, 999.9999999999998863 ) ;
#360 = CARTESIAN_POINT ( 'NONE',  ( -74.56250000000000000, 37.32233047033631124, 17.67766952966369232 ) ) ;
#361 = CARTESIAN_POINT ( 'NONE',  ( -72.12500000409677625, 55.00000000000000000, 24.99999999999999645 ) ) ;
#362 = AXIS2_PLACEMENT_3D ( 'NONE', #7929, #10661, #6136 ) ;
#363 = FACE_OUTER_BOUND ( 'NONE', #3792, .T. ) ;
#364 = VERTEX_POINT ( 'NONE', #1124 ) ;
#365 = EDGE_CURVE ( 'NONE', #1817, #1911, #2263, .T. ) ;
#366 = CARTESIAN_POINT ( 'NONE',  ( 5.249530852090826372, 48.30269735457433455, -2.031231156380094660 ) ) ;
#367 = DIRECTION ( 'NONE',  ( -0.000000000000000000, -1.000000000000000000, -0.000000000000000000 ) ) ;
#368 = CONICAL_SURFACE ( 'NONE', #5542, 2.500000000000000000, 0.9599310885968755924 ) ;
#369 = CARTESIAN_POINT ( 'NONE',  ( -78.00000000000001421, 59.24264068711928388, -12.72791868944003824 ) ) ;
#370 = CIRCLE ( 'NONE', #6328, 25.00000000000000355 ) ;
#371 = ORIENTED_EDGE ( 'NONE', *, *, #2057, .T. ) ;
#372 = CARTESIAN_POINT ( 'NONE',  ( 39.99999999999999289, 55.00000000000000000, 0.000000000000000000 ) ) ;
#373 = CARTESIAN_POINT ( 'NONE',  ( -75.96875000204839523, 73.25176868561975141, 18.25176868561974075 ) ) ;
#374 = ADVANCED_FACE ( 'NONE', ( #6893 ), #4791, .T. ) ;
#375 = ORIENTED_EDGE ( 'NONE', *, *, #453, .F. ) ;
#376 = CARTESIAN_POINT ( 'NONE',  ( -59.82750509709391196, 59.10995506582904824, 20.69284243654335498 ) ) ;
#377 = CARTESIAN_POINT ( 'NONE',  ( -75.03125000204839523, 36.74823131438024859, -18.25176868561973720 ) ) ;
#378 = CIRCLE ( 'NONE', #5553, 5.000000000000000888 ) ;
#379 = DIRECTION ( 'NONE',  ( 1.000000000000000000, 0.000000000000000000, 0.000000000000000000 ) ) ;
#380 = CARTESIAN_POINT ( 'NONE',  ( -59.59556320886013481, 52.94111634316250559, 20.93276532467568174 ) ) ;
#381 = CARTESIAN_POINT ( 'NONE',  ( -15.00000000000000355, 0.000000000000000000, 30.00000000000000711 ) ) ;
#382 = EDGE_CURVE ( 'NONE', #9787, #911, #6720, .T. ) ;
#383 = ORIENTED_EDGE ( 'NONE', *, *, #4826, .F. ) ;
#384 = CARTESIAN_POINT ( 'NONE',  ( -74.00000000204839523, 44.30836144126052289, 25.81189881250000795 ) ) ;
#385 = CARTESIAN_POINT ( 'NONE',  ( -80.00000000000000000, 55.00000000000000000, 24.99999999999999645 ) ) ;
#386 = VECTOR ( 'NONE', #9361, 1000.000000000000114 ) ;
#387 = CARTESIAN_POINT ( 'NONE',  ( -9.070746587277097817, 68.33487957594263662, -16.24597445391072270 ) ) ;
#388 = VERTEX_POINT ( 'NONE', #6780 ) ;
#389 = CARTESIAN_POINT ( 'NONE',  ( 18.18897147127288605, 67.92208482572254979, 16.80535131051722075 ) ) ;
#390 = CARTESIAN_POINT ( 'NONE',  ( -3.793771210778672298, 51.32715215846550905, -13.65164055122976983 ) ) ;
#391 = DIRECTION ( 'NONE',  ( 6.033820786006286457E-17, -1.000000000000000000, 0.000000000000000000 ) ) ;
#392 = CYLINDRICAL_SURFACE ( 'NONE', #7755, 1.499999999999999556 ) ;
#393 = VECTOR ( 'NONE', #8335, 1000.000000000000000 ) ;
#394 = UNCERTAINTY_MEASURE_WITH_UNIT (LENGTH_MEASURE( 1.000000000000000082E-05 ), #5013, 'distance_accuracy_value', 'NONE');
#395 = CARTESIAN_POINT ( 'NONE',  ( -78.00000000000002842, 42.27207793864211283, 5.742644059037075088 ) ) ;
#396 = ORIENTED_EDGE ( 'NONE', *, *, #10482, .T. ) ;
#397 = CARTESIAN_POINT ( 'NONE',  ( -77.37500000000000000, 30.00000000000000355, 4.592425496802573578E-15 ) ) ;
#398 = CARTESIAN_POINT ( 'NONE',  ( -2.450000000000000178, 3.000384657911015863E-16, -0.3851141460153411078 ) ) ;
#399 = CIRCLE ( 'NONE', #11681, 24.99999999999999645 ) ;
#400 = LINE ( 'NONE', #10690, #6493 ) ;
#401 = AXIS2_PLACEMENT_3D ( 'NONE', #2687, #9038, #3756 ) ;
#402 = CARTESIAN_POINT ( 'NONE',  ( -75.00000000000000000, 55.00000000000000000, 25.00000000000000355 ) ) ;
#403 = CARTESIAN_POINT ( 'NONE',  ( -32.20817489827727087, 48.19891751814265035, 1.703719440855944844 ) ) ;
#404 = ORIENTED_EDGE ( 'NONE', *, *, #2192, .T. ) ;
#405 = CARTESIAN_POINT ( 'NONE',  ( -27.49360061100878738, 37.45598436699922473, 11.71495266747331421 ) ) ;
#406 = CARTESIAN_POINT ( 'NONE',  ( 0.000000000000000000, 0.000000000000000000, -1.753742857142857048 ) ) ;
#407 = CARTESIAN_POINT ( 'NONE',  ( -1.648146632869006645, -4.821944789745371551, -9.959920860990531005E-16 ) ) ;
#408 = CARTESIAN_POINT ( 'NONE',  ( -75.31250000204839523, 29.18810118750000981, 10.69163855873950020 ) ) ;
#409 = DIRECTION ( 'NONE',  ( 0.000000000000000000, 0.000000000000000000, 1.000000000000000000 ) ) ;
#410 = CARTESIAN_POINT ( 'NONE',  ( -79.06250000204840944, 80.81189881250001861, -10.69163855873949132 ) ) ;
#411 = ORIENTED_EDGE ( 'NONE', *, *, #7065, .F. ) ;
#412 = CARTESIAN_POINT ( 'NONE',  ( -77.65625000409677625, 30.00000000000000355, -10.35533905932738108 ) ) ;
#413 = VECTOR ( 'NONE', #10435, 1000.000000000000114 ) ;
#414 = ORIENTED_EDGE ( 'NONE', *, *, #3400, .F. ) ;
#415 = CARTESIAN_POINT ( 'NONE',  ( -23.18906244097991021, 49.50939288222085821, 20.43027456479002879 ) ) ;
#416 = CLOSED_SHELL ( 'NONE', ( #7269, #9582, #2198, #63, #11043, #9304, #2244, #10765, #4629, #4313, #3244, #8345 ) ) ;
#417 = CARTESIAN_POINT ( 'NONE',  ( -79.34375000204839523, 73.25176868561975141, -18.25176868561974430 ) ) ;
#418 = PLANE ( 'NONE',  #9121 ) ;
#419 = CARTESIAN_POINT ( 'NONE',  ( -73.71875000000005684, 79.99999999999987210, -10.35533905932732424 ) ) ;
#420 = ORIENTED_EDGE ( 'NONE', *, *, #2126, .F. ) ;
#421 = CARTESIAN_POINT ( 'NONE',  ( -77.09374999999998579, 44.64466094067260826, -24.99999999999998934 ) ) ;
#422 = CARTESIAN_POINT ( 'NONE',  ( -72.03125000409679046, 44.64466094067262958, 25.00000000000001066 ) ) ;
#423 = SHAPE_REPRESENTATION ( 'Cast Iron Barrel & Hopper Casing', ( #4738 ), #3015 ) ;
#424 = CARTESIAN_POINT ( 'NONE',  ( -78.00000000000001421, 59.24264068711927678, -4.242637315201482906 ) ) ;
#425 = ORIENTED_EDGE ( 'NONE', *, *, #6952, .F. ) ;
#426 = EDGE_CURVE ( 'NONE', #7502, #11, #9516, .T. ) ;
#427 = ADVANCED_FACE ( 'NONE', ( #5819, #10408 ), #5935, .F. ) ;
#428 = CARTESIAN_POINT ( 'NONE',  ( -8.750920173525754464, 61.18660372065389907, -3.306409054201195907 ) ) ;
#429 = CARTESIAN_POINT ( 'NONE',  ( 0.000000000000000000, 0.000000000000000000, 0.000000000000000000 ) ) ;
#430 = VERTEX_POINT ( 'NONE', #4072 ) ;
#431 = CARTESIAN_POINT ( 'NONE',  ( 10.64984185237921466, 68.68279778901450072, -17.23294504368761793 ) ) ;
#432 = EDGE_CURVE ( 'NONE', #3322, #5122, #11360, .T. ) ;
#433 = CARTESIAN_POINT ( 'NONE',  ( -78.87500000204839523, 65.69163855873949842, 25.81189881250000084 ) ) ;
#434 = ORIENTED_EDGE ( 'NONE', *, *, #8927, .T. ) ;
#435 = CARTESIAN_POINT ( 'NONE',  ( -42.92935705524211443, 57.05913440163546113, -20.93112575922673102 ) ) ;
#436 = CARTESIAN_POINT ( 'NONE',  ( -72.68750000204839523, 65.69163855873949842, 25.81189881250000440 ) ) ;
#437 = ADVANCED_FACE ( 'NONE', ( #8976 ), #2509, .T. ) ;
#438 = EDGE_CURVE ( 'NONE', #9864, #879, #4301, .T. ) ;
#439 = EDGE_CURVE ( 'NONE', #8561, #9242, #6055, .T. ) ;
#440 = DIRECTION ( 'NONE',  ( 0.000000000000000000, 1.000000000000000000, 0.000000000000000000 ) ) ;
#441 = CARTESIAN_POINT ( 'NONE',  ( -78.00000000000001421, 59.24264068711927678, -4.242637315201482906 ) ) ;
#442 = CARTESIAN_POINT ( 'NONE',  ( -78.00000000000001421, 59.24264068711927678, 5.742644059037073312 ) ) ;
#443 = VERTEX_POINT ( 'NONE', #7009 ) ;
#444 = CARTESIAN_POINT ( 'NONE',  ( -5.000000000000000000, -2.886751345948134428, -0.4465819873852071575 ) ) ;
#445 = EDGE_CURVE ( 'NONE', #3923, #1810, #7380, .T. ) ;
#446 = CARTESIAN_POINT ( 'NONE',  ( -32.99614454614441428, 33.97685596767119165, 0.0005149883856687357403 ) ) ;
#447 = EDGE_CURVE ( 'NONE', #3965, #2443, #10013, .T. ) ;
#448 = ORIENTED_EDGE ( 'NONE', *, *, #1072, .T. ) ;
#449 = CARTESIAN_POINT ( 'NONE',  ( -60.26222962708032327, 52.94112624030389469, 20.93216173895077503 ) ) ;
#450 = CARTESIAN_POINT ( 'NONE',  ( -25.53957388397973105, 51.34093700237838931, 13.61837799178155350 ) ) ;
#451 = CARTESIAN_POINT ( 'NONE',  ( -78.87500000000002842, 30.00000000000003553, 4.592425496802568845E-15 ) ) ;
#452 = DIRECTION ( 'NONE',  ( -1.000000000000000000, -0.000000000000000000, -0.000000000000000000 ) ) ;
#453 = EDGE_CURVE ( 'NONE', #5713, #10987, #3706, .T. ) ;
#454 = CARTESIAN_POINT ( 'NONE',  ( -73.62500000409677625, 55.00000000000000000, 24.99999999999999645 ) ) ;
#455 = ORIENTED_EDGE ( 'NONE', *, *, #1627, .F. ) ;
#456 = CARTESIAN_POINT ( 'NONE',  ( -72.78125000000002842, 30.00000000000000355, -10.35533905932738108 ) ) ;
#457 = CARTESIAN_POINT ( 'NONE',  ( -64.61922394917361601, 54.99794615529658159, 0.004759334053694205813 ) ) ;
#458 = VECTOR ( 'NONE', #2991, 1000.000000000000000 ) ;
#459 = DIRECTION ( 'NONE',  ( 1.000000000000000000, -0.000000000000000000, -0.000000000000000000 ) ) ;
#460 = CARTESIAN_POINT ( 'NONE',  ( -78.00000000000000000, 54.99999999999999289, 1.500003371917797201 ) ) ;
#461 = CARTESIAN_POINT ( 'NONE',  ( -22.00013559226026771, 57.68156399829890546, 6.473040822733857169 ) ) ;
#462 = ORIENTED_EDGE ( 'NONE', *, *, #11425, .T. ) ;
#463 = CARTESIAN_POINT ( 'NONE',  ( -30.40408068685511367, 34.08504365610654219, 2.058398070974400529 ) ) ;
#464 = FACE_OUTER_BOUND ( 'NONE', #2972, .T. ) ;
#465 = DIRECTION ( 'NONE',  ( 0.000000000000000000, 0.000000000000000000, 1.000000000000000000 ) ) ;
#466 = CARTESIAN_POINT ( 'NONE',  ( -77.09375000204839523, 55.00000000000000000, 25.81189881249999729 ) ) ;
#467 = CARTESIAN_POINT ( 'NONE',  ( -11.05058114698192107, 69.12285606448547526, 20.64999657351882689 ) ) ;
#468 = CARTESIAN_POINT ( 'NONE',  ( -75.31250000204839523, 29.18810118750000981, 10.69163855873950020 ) ) ;
#469 = ORIENTED_EDGE ( 'NONE', *, *, #6959, .T. ) ;
#470 = CARTESIAN_POINT ( 'NONE',  ( -76.34375000409680467, 30.00000000000001421, 10.35533905932739174 ) ) ;
#471 = FACE_OUTER_BOUND ( 'NONE', #3888, .T. ) ;
#472 = FACE_BOUND ( 'NONE', #918, .T. ) ;
#473 = CARTESIAN_POINT ( 'NONE',  ( -7.070747353360942178, 68.33360022464046324, -16.24461469319379603 ) ) ;
#474 = CARTESIAN_POINT ( 'NONE',  ( -75.21875000000007105, 79.99999999999990052, -10.35533905932733134 ) ) ;
#475 = DIRECTION ( 'NONE',  ( 0.000000000000000000, 0.000000000000000000, 1.000000000000000000 ) ) ;
#476 = LINE ( 'NONE', #4199, #9328 ) ;
#477 = STYLED_ITEM ( 'NONE', ( #10437 ), #9416 ) ;
#478 =( GEOMETRIC_REPRESENTATION_CONTEXT ( 3 ) GLOBAL_UNCERTAINTY_ASSIGNED_CONTEXT ( ( #4789 ) ) GLOBAL_UNIT_ASSIGNED_CONTEXT ( ( #10005, #10508, #11461 ) ) REPRESENTATION_CONTEXT ( 'NONE', 'WORKASPACE' ) );
#479 = EDGE_LOOP ( 'NONE', ( #6589, #1548 ) ) ;
#480 = CARTESIAN_POINT ( 'NONE',  ( -79.25000000000000000, 55.00000000000000000, 24.99999999999999645 ) ) ;
#481 = CARTESIAN_POINT ( 'NONE',  ( -72.21875000000001421, 80.00000000000001421, -10.35533905932737753 ) ) ;
#482 = DIRECTION ( 'NONE',  ( -9.813077866773612233E-16, 1.000000000000000000, 0.000000000000000000 ) ) ;
#483 = DIRECTION ( 'NONE',  ( -0.000000000000000000, -0.000000000000000000, -1.000000000000000000 ) ) ;
#484 = ORIENTED_EDGE ( 'NONE', *, *, #797, .F. ) ;
#485 = EDGE_CURVE ( 'NONE', #7813, #9573, #2446, .T. ) ;
#486 = CARTESIAN_POINT ( 'NONE',  ( -60.95809730739352261, 51.99959260526208737, 6.342595581606403243 ) ) ;
#487 = CARTESIAN_POINT ( 'NONE',  ( -78.12500000409677625, 55.00000000000000000, 24.99999999999999645 ) ) ;
#488 = LINE ( 'NONE', #11560, #10630 ) ;
#489 = PRODUCT_DEFINITION_SHAPE ( 'NONE', 'NONE',  #9810 ) ;
#490 = AXIS2_PLACEMENT_3D ( 'NONE', #6892, #11533, #10461 ) ;
#491 = EDGE_LOOP ( 'NONE', ( #6034, #9162, #10252, #4142 ) ) ;
#492 = CARTESIAN_POINT ( 'NONE',  ( 21.70367235178696319, 76.99085433373973331, 0.7325029477543631984 ) ) ;
#493 = CARTESIAN_POINT ( 'NONE',  ( -77.84375000204839523, 73.25176868561975141, -18.25176868561974430 ) ) ;
#494 = VERTEX_POINT ( 'NONE', #7845 ) ;
#495 = CARTESIAN_POINT ( 'NONE',  ( -72.03125000204839523, 36.74823131438024859, -18.25176868561973720 ) ) ;
#496 = LINE ( 'NONE', #7937, #10551 ) ;
#497 = CARTESIAN_POINT ( 'NONE',  ( 10.42614132098574586, 55.02481535990867911, -0.008496357143309388182 ) ) ;
#498 = CARTESIAN_POINT ( 'NONE',  ( 0.000000000000000000, 0.000000000000000000, -2.968018054819144158 ) ) ;
#499 = COLOUR_RGB ( '',0.8941176470588234615, 0.8941176470588234615, 0.8941176470588234615 ) ;
#500 = ORIENTED_EDGE ( 'NONE', *, *, #3520, .F. ) ;
#501 = CARTESIAN_POINT ( 'NONE',  ( -41.16026710375170694, 50.89060761561553647, -20.69263693287480521 ) ) ;
#502 = ORIENTED_EDGE ( 'NONE', *, *, #10815, .T. ) ;
#503 = CARTESIAN_POINT ( 'NONE',  ( -68.19377681732581209, 34.02207046653818168, 2.749122354329981643 ) ) ;
#504 = CARTESIAN_POINT ( 'NONE',  ( -41.49691193415848289, 52.26032216745779380, -13.79378832249819986 ) ) ;
#505 = CARTESIAN_POINT ( 'NONE',  ( -2.500000000000000000, 3.061616997868383141E-16, -2.103846626247716234 ) ) ;
#506 = AXIS2_PLACEMENT_3D ( 'NONE', #833, #7216, #2766 ) ;
#507 = CARTESIAN_POINT ( 'NONE',  ( -27.14812531749841895, 52.78402274155275364, 4.494092492992627363 ) ) ;
#508 = CONICAL_SURFACE ( 'NONE', #1852, 3.000000000000000000, 0.9599310885968912466 ) ;
#509 = ORIENTED_EDGE ( 'NONE', *, *, #11168, .T. ) ;
#510 = CARTESIAN_POINT ( 'NONE',  ( -74.18750000000000000, 37.32233047033631124, -17.67766952966368166 ) ) ;
#511 = CARTESIAN_POINT ( 'NONE',  ( -69.75702627179666138, 54.98186149566993208, 0.007223337549123830421 ) ) ;
#512 = ADVANCED_FACE ( 'NONE', ( #9745 ), #11473, .F. ) ;
#513 = CYLINDRICAL_SURFACE ( 'NONE', #1318, 1.499999999999999556 ) ;
#514 = CIRCLE ( 'NONE', #703, 2.999999999999995559 ) ;
#515 = CYLINDRICAL_SURFACE ( 'NONE', #11802, 29.00000000000000355 ) ;
#516 = CARTESIAN_POINT ( 'NONE',  ( -50.77658096445664171, 61.83369931620287474, -1.838789935413423171 ) ) ;
#517 = AXIS2_PLACEMENT_3D ( 'NONE', #9788, #1581, #2488 ) ;
#518 = VERTEX_POINT ( 'NONE', #5210 ) ;
#519 = CARTESIAN_POINT ( 'NONE',  ( -54.32961274566940801, 69.86573439484330095, 14.86481071665870601 ) ) ;
#520 = DIRECTION ( 'NONE',  ( -1.000000000000000000, 0.000000000000000000, 0.000000000000000000 ) ) ;
#521 = CARTESIAN_POINT ( 'NONE',  ( 2.287832656137188447, -4.452621892014644978, -5.917583927755353772E-16 ) ) ;
#522 = EDGE_CURVE ( 'NONE', #2578, #3782, #9633, .T. ) ;
#523 = CARTESIAN_POINT ( 'NONE',  ( -79.06250000204840944, 80.81189881250000440, -10.69163855873948954 ) ) ;
#524 = CARTESIAN_POINT ( 'NONE',  ( -1.708601562010274133, 65.50638515368892456, 22.68572929305231867 ) ) ;
#525 = CARTESIAN_POINT ( 'NONE',  ( -76.62500000204839523, 29.18810118750000626, -10.69163855873949309 ) ) ;
#526 = ORIENTED_EDGE ( 'NONE', *, *, #1693, .F. ) ;
#527 = CARTESIAN_POINT ( 'NONE',  ( -74.37500000409677625, 55.00000000000000000, -24.99999999999999645 ) ) ;
#528 = FACE_BOUND ( 'NONE', #6654, .T. ) ;
#529 = CARTESIAN_POINT ( 'NONE',  ( -75.49999999999972999, 55.00000000002793854, -24.99999999999999645 ) ) ;
#530 = AXIS2_PLACEMENT_3D ( 'NONE', #8639, #9703, #5223 ) ;
#531 = CARTESIAN_POINT ( 'NONE',  ( -5.030643890195627854, 62.08057558410310861, -19.78873666113293694 ) ) ;
#532 = CARTESIAN_POINT ( 'NONE',  ( -77.84375000204839523, 73.25176868561975141, -18.25176868561974430 ) ) ;
#533 = CARTESIAN_POINT ( 'NONE',  ( -20.00000000000003197, -63.00000000000000000, 5.000000000000000000 ) ) ;
#534 = DIRECTION ( 'NONE',  ( -1.000000000000000000, 0.000000000000000000, 0.000000000000000000 ) ) ;
#535 = CONICAL_SURFACE ( 'NONE', #9339, 3.000000000000000000, 0.9599310885968912466 ) ;
#536 = ORIENTED_EDGE ( 'NONE', *, *, #5953, .F. ) ;
#537 = DIRECTION ( 'NONE',  ( -1.000000000000000000, -0.000000000000000000, -0.000000000000000000 ) ) ;
#538 = CARTESIAN_POINT ( 'NONE',  ( -74.75000000000000000, 55.00000000000000000, 24.99999999999999645 ) ) ;
#539 = DIRECTION ( 'NONE',  ( -1.000000000000000000, -6.033820786006286457E-17, -0.000000000000000000 ) ) ;
#540 = CYLINDRICAL_SURFACE ( 'NONE', #2889, 1.499999999999999556 ) ;
#541 = VERTEX_POINT ( 'NONE', #1428 ) ;
#542 = EDGE_CURVE ( 'NONE', #5255, #5411, #11153, .T. ) ;
#543 = CARTESIAN_POINT ( 'NONE',  ( -53.95794482029891981, 59.71207155077219397, 5.199202863523991525 ) ) ;
#544 = CARTESIAN_POINT ( 'NONE',  ( -78.50000000409677625, 80.00000000000000000, -1.530808498934191324E-15 ) ) ;
#545 = SURFACE_STYLE_USAGE ( .BOTH. , #6919 ) ;
#546 = VERTEX_POINT ( 'NONE', #9861 ) ;
#547 = CARTESIAN_POINT ( 'NONE',  ( 2.917962331683024768, 65.29045701389995315, -19.44540138122387773 ) ) ;
#548 = DIRECTION ( 'NONE',  ( -1.000000000000000000, -0.000000000000000000, -0.000000000000000000 ) ) ;
#549 = ORIENTED_EDGE ( 'NONE', *, *, #6671, .F. ) ;
#550 = CARTESIAN_POINT ( 'NONE',  ( -78.03125000204839523, 36.74823131438024859, -18.25176868561973720 ) ) ;
#551 = FACE_OUTER_BOUND ( 'NONE', #562, .T. ) ;
#552 = CARTESIAN_POINT ( 'NONE',  ( -75.40625000409677625, 80.00000000000001421, 10.35533905932737397 ) ) ;
#553 = CARTESIAN_POINT ( 'NONE',  ( -18.33546440020741741, 54.99907998473290149, -0.002823738427829867569 ) ) ;
#554 = AXIS2_PLACEMENT_3D ( 'NONE', #4747, #2103, #5776 ) ;
#555 = DIRECTION ( 'NONE',  ( 0.000000000000000000, 0.000000000000000000, 1.000000000000000000 ) ) ;
#556 = VECTOR ( 'NONE', #11155, 1000.000000000000000 ) ;
#557 = CARTESIAN_POINT ( 'NONE',  ( -75.00000000000004263, 38.53867536077979139, -19.88773376194887987 ) ) ;
#558 = ADVANCED_FACE ( 'NONE', ( #7904 ), #1983, .F. ) ;
#559 = ORIENTED_EDGE ( 'NONE', *, *, #6186, .F. ) ;
#560 = DIRECTION ( 'NONE',  ( -1.000000000000000000, -0.000000000000000000, -0.000000000000000000 ) ) ;
#561 = CARTESIAN_POINT ( 'NONE',  ( -40.60828084101493829, 48.86090744392433294, -20.20262880343927847 ) ) ;
#562 = EDGE_LOOP ( 'NONE', ( #8719, #3480, #10235, #11530 ) ) ;
#563 = CARTESIAN_POINT ( 'NONE',  ( -60.92889604530372338, 52.94113613744689673, 20.93155815322914393 ) ) ;
#564 = CARTESIAN_POINT ( 'NONE',  ( -11.16981900506391234, 66.69595144640879880, -7.821387473301188997 ) ) ;
#565 = CARTESIAN_POINT ( 'NONE',  ( -74.18750000204838102, 44.30836144126053000, 25.81189881250000795 ) ) ;
#566 = AXIS2_PLACEMENT_3D ( 'NONE', #8644, #10369, #4811 ) ;
#567 = VERTEX_POINT ( 'NONE', #5147 ) ;
#568 = CARTESIAN_POINT ( 'NONE',  ( -73.25000000000000000, 55.00000000000000000, 24.99999999999999645 ) ) ;
#569 = CARTESIAN_POINT ( 'NONE',  ( 16.47760469315713294, 57.74566955740679930, 20.97627666568605420 ) ) ;
#570 = ADVANCED_FACE ( 'NONE', ( #3399 ), #11717, .F. ) ;
#571 = ORIENTED_EDGE ( 'NONE', *, *, #3449, .F. ) ;
#572 = AXIS2_PLACEMENT_3D ( 'NONE', #3732, #4757, #2835 ) ;
#573 = CARTESIAN_POINT ( 'NONE',  ( 19.14254474247333349, 57.21240123512449571, 4.495849551821894607 ) ) ;
#574 = CARTESIAN_POINT ( 'NONE',  ( -25.10988330751693809, 54.08371348254146938, 7.017189493341159157 ) ) ;
#575 = ORIENTED_EDGE ( 'NONE', *, *, #6777, .T. ) ;
#576 = CARTESIAN_POINT ( 'NONE',  ( -36.47762819585614835, 42.07544065584382764, -16.80749884933775462 ) ) ;
#577 = AXIS2_PLACEMENT_3D ( 'NONE', #3496, #11567, #2539 ) ;
#578 = DIRECTION ( 'NONE',  ( -0.000000000000000000, -0.000000000000000000, -1.000000000000000000 ) ) ;
#579 = CARTESIAN_POINT ( 'NONE',  ( 52.99999999999999289, 58.53553390593273065, -3.535533905932738197 ) ) ;
#580 = CARTESIAN_POINT ( 'NONE',  ( -77.46875000204839523, 80.81189881250000440, -1.580522963032174394E-15 ) ) ;
#581 = DIRECTION ( 'NONE',  ( -1.000000000000000000, -0.000000000000000000, -0.000000000000000000 ) ) ;
#582 = CARTESIAN_POINT ( 'NONE',  ( -73.15625000204839523, 73.25176868561975141, -18.25176868561974430 ) ) ;
#583 = EDGE_LOOP ( 'NONE', ( #10142, #10451 ) ) ;
#584 = CARTESIAN_POINT ( 'NONE',  ( -75.12500000409677625, 55.00000000000000000, 24.99999999999999645 ) ) ;
#585 = DIRECTION ( 'NONE',  ( -1.000000000000000000, -0.000000000000000000, -0.000000000000000000 ) ) ;
#586 = CARTESIAN_POINT ( 'NONE',  ( -71.56250000409677625, 37.32233047033631124, -17.67766952966368166 ) ) ;
#587 = EDGE_CURVE ( 'NONE', #96, #430, #9252, .T. ) ;
#588 = CARTESIAN_POINT ( 'NONE',  ( -18.73741402030934111, 64.90551912913463184, 18.53518525054827393 ) ) ;
#589 = EDGE_CURVE ( 'NONE', #6548, #8998, #260, .T. ) ;
#590 = VECTOR ( 'NONE', #3641, 1000.000000000000000 ) ;
#591 = ORIENTED_EDGE ( 'NONE', *, *, #3891, .F. ) ;
#592 = AXIS2_PLACEMENT_3D ( 'NONE', #1916, #1680, #10056 ) ;
#593 = CARTESIAN_POINT ( 'NONE',  ( 36.99999999999999289, 55.00000000000000000, 0.000000000000000000 ) ) ;
#594 = CARTESIAN_POINT ( 'NONE',  ( 39.99999999999999289, 55.00000000000000000, 0.000000000000000000 ) ) ;
#595 = DIRECTION ( 'NONE',  ( 0.000000000000000000, 0.000000000000000000, -1.000000000000000000 ) ) ;
#596 = CARTESIAN_POINT ( 'NONE',  ( 0.000000000000000000, 0.000000000000000000, -5.560532340533429263 ) ) ;
#597 = AXIS2_PLACEMENT_3D ( 'NONE', #6359, #1665, #761 ) ;
#598 = CARTESIAN_POINT ( 'NONE',  ( -78.03125000204838102, 55.00000000000000000, -25.81189881249999729 ) ) ;
#599 = AXIS2_PLACEMENT_3D ( 'NONE', #5358, #1631, #1752 ) ;
#600 = CYLINDRICAL_SURFACE ( 'NONE', #4784, 1.499999999999999556 ) ;
#601 = ORIENTED_EDGE ( 'NONE', *, *, #9027, .F. ) ;
#602 = EDGE_CURVE ( 'NONE', #4836, #8743, #10811, .T. ) ;
#603 = DIRECTION ( 'NONE',  ( 1.000000000000000000, 0.000000000000000000, 0.000000000000000000 ) ) ;
#604 = B_SPLINE_CURVE_WITH_KNOTS ( 'NONE', 3,
 ( #3860, #10555, #7751, #4149, #4093, #7812, #1399, #3253 ),
 .UNSPECIFIED., .F., .F.,
 ( 4, 2, 2, 4 ),
 ( 0.002921158011986710757, 0.003648658599403066180, 0.004376159186819420302, 0.005831160361652131148 ),
 .UNSPECIFIED. ) ;
#605 = EDGE_LOOP ( 'NONE', ( #2787, #4447, #826, #2747 ) ) ;
#606 = CARTESIAN_POINT ( 'NONE',  ( -49.58248963817779753, 62.01904108894438394, 0.6873064985993181386 ) ) ;
#607 = CARTESIAN_POINT ( 'NONE',  ( 47.00000000000000000, 55.00000000000000000, 0.000000000000000000 ) ) ;
#608 = CARTESIAN_POINT ( 'NONE',  ( -1.653121499799246052, 4.819072548984003390, -0.05140428708382603629 ) ) ;
#609 = CYLINDRICAL_SURFACE ( 'NONE', #11207, 2.500000000000000000 ) ;
#610 = VECTOR ( 'NONE', #11628, 1000.000000000000000 ) ;
#611 = CARTESIAN_POINT ( 'NONE',  ( 12.31292331232940640, 69.75642766769821890, 16.32415115763334867 ) ) ;
#612 = CARTESIAN_POINT ( 'NONE',  ( -72.12500000204839523, 44.30836144126049447, -25.81189881249999019 ) ) ;
#613 = ORIENTED_EDGE ( 'NONE', *, *, #643, .T. ) ;
#614 = CARTESIAN_POINT ( 'NONE',  ( -76.62500000204839523, 29.18810118750000626, -10.69163855873949309 ) ) ;
#615 = DIRECTION ( 'NONE',  ( -1.000000000000000000, -0.000000000000000000, -0.000000000000000000 ) ) ;
#616 = FACE_BOUND ( 'NONE', #1270, .T. ) ;
#617 = CARTESIAN_POINT ( 'NONE',  ( 25.99999999999999645, 54.99999999999999289, 0.000000000000000000 ) ) ;
#618 = CARTESIAN_POINT ( 'NONE',  ( -74.99999999999997158, 37.75762616273102168, -19.19216994046665903 ) ) ;
#619 = EDGE_LOOP ( 'NONE', ( #3574, #9268, #7450, #6908 ) ) ;
#620 = CARTESIAN_POINT ( 'NONE',  ( -29.45688395272410887, 50.03307866788530589, 0.6599468027641450796 ) ) ;
#621 = CARTESIAN_POINT ( 'NONE',  ( -42.03064326886630653, 53.96872019721284630, -20.99365203016559178 ) ) ;
#622 = ORIENTED_EDGE ( 'NONE', *, *, #9614, .F. ) ;
#623 = CARTESIAN_POINT ( 'NONE',  ( -45.17314290467847115, 66.71834769317766245, -17.55197735385382174 ) ) ;
#624 = CARTESIAN_POINT ( 'NONE',  ( -30.70300456119418797, 42.33444820903851991, 5.990538379293029791 ) ) ;
#625 = CARTESIAN_POINT ( 'NONE',  ( -77.75000000204839523, 80.81189881250001861, -10.69163855873949132 ) ) ;
#626 = ORIENTED_EDGE ( 'NONE', *, *, #8896, .F. ) ;
#627 = CARTESIAN_POINT ( 'NONE',  ( -73.90625000000001421, 65.35533905932737753, -24.99999999999999645 ) ) ;
#628 = LINE ( 'NONE', #2373, #1454 ) ;
#629 = ADVANCED_FACE ( 'NONE', ( #7359 ), #4594, .T. ) ;
#630 =( BOUNDED_CURVE ( )  B_SPLINE_CURVE ( 2, ( #7577, #9479, #6681, #10311, #8593, #2108, #3973, #5782, #1209 ),
 .UNSPECIFIED., .F., .T. ) 
 B_SPLINE_CURVE_WITH_KNOTS ( ( 3, 2, 2, 2, 3 ),
 ( 0.7129436809910058015, 0.7327527857159548130, 0.7525618904409037135, 0.7723709951658527251, 0.7921800998908017366 ),
 .UNSPECIFIED. ) 
 CURVE ( )  GEOMETRIC_REPRESENTATION_ITEM ( )  RATIONAL_B_SPLINE_CURVE ( ( 1.000000000000000000, 0.9238795325112866275, 1.000000000000000000, 0.9238795325112866275, 1.000000000000000000, 0.9238795325112866275, 1.000000000000000000, 0.9238795325112866275, 1.000000000000000000 ) ) 
 REPRESENTATION_ITEM ( '' )  );
#631 = ORIENTED_EDGE ( 'NONE', *, *, #4619, .T. ) ;
#632 = CARTESIAN_POINT ( 'NONE',  ( 0.000000000000000000, 0.000000000000000000, -6.099999999999999645 ) ) ;
#633 = CARTESIAN_POINT ( 'NONE',  ( 0.000000000000000000, -30.00000000000000000, 0.000000000000000000 ) ) ;
#634 = CARTESIAN_POINT ( 'NONE',  ( -11.49982872529378852, 60.84893598204366327, -3.911509378443825291 ) ) ;
#635 = EDGE_LOOP ( 'NONE', ( #794, #9910 ) ) ;
#636 = CARTESIAN_POINT ( 'NONE',  ( -61.63584152524990145, 46.00569487729882212, 19.01260273971552905 ) ) ;
#637 = CARTESIAN_POINT ( 'NONE',  ( 19.14436220527237253, 71.77763100192429135, 12.89423484158165500 ) ) ;
#638 = DIRECTION ( 'NONE',  ( -1.000000000000000000, 0.000000000000000000, 0.000000000000000000 ) ) ;
#639 = ADVANCED_FACE ( 'NONE', ( #8250 ), #10934, .T. ) ;
#640 = CARTESIAN_POINT ( 'NONE',  ( -78.00000000000002842, 46.51471862576140381, 1.500003371917798756 ) ) ;
#641 = CARTESIAN_POINT ( 'NONE',  ( -74.93750000204839523, 44.30836144126050158, -25.81189881249999374 ) ) ;
#642 = VERTEX_POINT ( 'NONE', #2683 ) ;
#643 = EDGE_CURVE ( 'NONE', #9312, #7093, #6230, .T. ) ;
#644 = CARTESIAN_POINT ( 'NONE',  ( -71.37500000409677625, 55.00000000000000000, -24.99999999999999645 ) ) ;
#645 = DIRECTION ( 'NONE',  ( 0.000000000000000000, 0.000000000000000000, -1.000000000000000000 ) ) ;
#646 = DIRECTION ( 'NONE',  ( 0.000000000000000000, 0.000000000000000000, 1.000000000000000000 ) ) ;
#647 = CARTESIAN_POINT ( 'NONE',  ( 14.85570562722353749, 52.25434861561973321, 21.02374011750137939 ) ) ;
#648 = ORIENTED_EDGE ( 'NONE', *, *, #111, .F. ) ;
#649 = CARTESIAN_POINT ( 'NONE',  ( -75.87500000204838102, 65.69163855873949842, 25.81189881250000084 ) ) ;
#650 = CARTESIAN_POINT ( 'NONE',  ( -78.00000000000000000, 54.99999999999999289, 3.371917797062584654E-06 ) ) ;
#651 = DIRECTION ( 'NONE',  ( -0.000000000000000000, -0.000000000000000000, -1.000000000000000000 ) ) ;
#652 = CARTESIAN_POINT ( 'NONE',  ( -32.11869219899978845, 34.20636958863568822, 3.085052597841025701 ) ) ;
#653 = CARTESIAN_POINT ( 'NONE',  ( 2.500000000000000000, 0.000000000000000000, -4.696360911962001339 ) ) ;
#654 = CARTESIAN_POINT ( 'NONE',  ( -74.84375000204839523, 73.25176868561975141, -18.25176868561974430 ) ) ;
#655 = CYLINDRICAL_SURFACE ( 'NONE', #8229, 5.000000000000000000 ) ;
#656 = VERTEX_POINT ( 'NONE', #1719 ) ;
#657 = CARTESIAN_POINT ( 'NONE',  ( 0.000000000000000000, -57.00000000000000000, 0.000000000000000000 ) ) ;
#658 = VERTEX_POINT ( 'NONE', #3636 ) ;
#659 = CARTESIAN_POINT ( 'NONE',  ( -66.89547590671475064, 48.02433609231711387, 0.9101378528334346241 ) ) ;
#660 = ADVANCED_FACE ( 'NONE', ( #2854 ), #866, .F. ) ;
#661 = CARTESIAN_POINT ( 'NONE',  ( -71.34302368722835297, 77.35376350879521112, 12.90594348738575903 ) ) ;
#662 = CARTESIAN_POINT ( 'NONE',  ( 53.00000000000000000, 47.00000000000000711, -6.000000000000000000 ) ) ;
#663 = COLOUR_RGB ( '',1.000000000000000000, 0.9490196078431372140, 0.9098039215686274384 ) ;
#664 = CARTESIAN_POINT ( 'NONE',  ( 20.82597707344048743, 76.25689989831184334, -5.711711607058635565 ) ) ;
#665 = CARTESIAN_POINT ( 'NONE',  ( -71.93750000204838102, 65.69163855873948421, -25.81189881250000084 ) ) ;
#666 = ORIENTED_EDGE ( 'NONE', *, *, #2138, .F. ) ;
#667 = CARTESIAN_POINT ( 'NONE',  ( -74.84375000204839523, 55.00000000000000000, -25.81189881249999729 ) ) ;
#668 = EDGE_CURVE ( 'NONE', #7145, #5117, #992, .T. ) ;
#669 = CARTESIAN_POINT ( 'NONE',  ( -78.00000000000001421, 63.48528137423857487, 3.371917795327861178E-06 ) ) ;
#670 = UNCERTAINTY_MEASURE_WITH_UNIT (LENGTH_MEASURE( 1.000000000000000082E-05 ), #7474, 'distance_accuracy_value', 'NONE');
#671 = CARTESIAN_POINT ( 'NONE',  ( 0.000000000000000000, 0.000000000000000000, -6.099999999999999645 ) ) ;
#672 = CARTESIAN_POINT ( 'NONE',  ( 22.90732450365403849, 55.02356608025330331, 0.01155963734724412169 ) ) ;
#673 = CARTESIAN_POINT ( 'NONE',  ( 0.000000000000000000, 0.000000000000000000, 0.000000000000000000 ) ) ;
#674 = CARTESIAN_POINT ( 'NONE',  ( -74.99999999999998579, 36.28446816562487243, -17.71219965803775764 ) ) ;
#675 = ORIENTED_EDGE ( 'NONE', *, *, #799, .F. ) ;
#676 = FACE_OUTER_BOUND ( 'NONE', #7285, .T. ) ;
#677 = CARTESIAN_POINT ( 'NONE',  ( -54.59603348275399526, 73.54984634329692028, 9.912388241271610667 ) ) ;
#678 = VERTEX_POINT ( 'NONE', #4538 ) ;
#679 = CARTESIAN_POINT ( 'NONE',  ( -23.81092923484322199, 52.25445676425606223, 21.02046492383515641 ) ) ;
#680 = CARTESIAN_POINT ( 'NONE',  ( -44.99813998784102154, 60.36285607543581477, -12.94816624433304142 ) ) ;
#681 = CARTESIAN_POINT ( 'NONE',  ( -79.25000000204838102, 80.81189881250001861, -10.69163855873949132 ) ) ;
#682 = CIRCLE ( 'NONE', #1258, 2.445500000000003116 ) ;
#683 = ORIENTED_EDGE ( 'NONE', *, *, #522, .T. ) ;
#684 = MANIFOLD_SOLID_BREP ( 'M6 Machine Threads Stud1', #2327 ) ;
#685 = CARTESIAN_POINT ( 'NONE',  ( -71.95822497812569907, 74.53807824654330716, 16.15905817987090032 ) ) ;
#686 = CARTESIAN_POINT ( 'NONE',  ( 47.00000000000000000, 47.00000000000000711, 6.000000000000000000 ) ) ;
#687 = AXIS2_PLACEMENT_3D ( 'NONE', #9704, #7974, #8697 ) ;
#688 = CARTESIAN_POINT ( 'NONE',  ( -78.00000000000001421, 71.97056274847716395, 3.371917795327861178E-06 ) ) ;
#689 = CARTESIAN_POINT ( 'NONE',  ( -80.00000000000000000, 55.00000000000000000, -24.99999999999999645 ) ) ;
#690 = CARTESIAN_POINT ( 'NONE',  ( -70.99971551311861617, 47.99600105715470733, 0.0002324378226963109213 ) ) ;
#691 = ORIENTED_EDGE ( 'NONE', *, *, #8944, .T. ) ;
#692 = CARTESIAN_POINT ( 'NONE',  ( -61.32723930490969622, 46.95308112547827051, 19.41976192622660946 ) ) ;
#693 = VECTOR ( 'NONE', #6124, 1000.000000000000000 ) ;
#694 = CARTESIAN_POINT ( 'NONE',  ( -74.99999999999998579, 39.36515909056227258, -20.53791299142420712 ) ) ;
#695 = CARTESIAN_POINT ( 'NONE',  ( 1.443735181952764624, -4.939961795957305668, -0.08165819712377517248 ) ) ;
#696 = FACE_OUTER_BOUND ( 'NONE', #7625, .T. ) ;
#697 = DIRECTION ( 'NONE',  ( 0.000000000000000000, 1.000000000000000000, 0.000000000000000000 ) ) ;
#698 = ORIENTED_EDGE ( 'NONE', *, *, #6458, .F. ) ;
#699 = CARTESIAN_POINT ( 'NONE',  ( -74.28125000409676204, 65.35533905932737753, -24.99999999999999645 ) ) ;
#700 = DIRECTION ( 'NONE',  ( -1.000000000000000000, -0.000000000000000000, -0.000000000000000000 ) ) ;
#701 = LINE ( 'NONE', #8025, #1937 ) ;
#702 = CARTESIAN_POINT ( 'NONE',  ( -54.63607242817042930, 69.12530316040908929, 15.58420556269393309 ) ) ;
#703 = AXIS2_PLACEMENT_3D ( 'NONE', #8408, #9360, #5659 ) ;
#704 = ORIENTED_EDGE ( 'NONE', *, *, #10995, .F. ) ;
#705 = CARTESIAN_POINT ( 'NONE',  ( -75.03125000204838102, 55.00000000000000000, -25.81189881249999729 ) ) ;
#706 = CIRCLE ( 'NONE', #5497, 5.000000000000000000 ) ;
#707 = CARTESIAN_POINT ( 'NONE',  ( -15.00000000000000355, 5.000000000000000000, 30.00000000000000711 ) ) ;
#708 = CARTESIAN_POINT ( 'NONE',  ( -71.53052369147287948, 77.35376373433385311, 12.90594309674112772 ) ) ;
#709 = DIRECTION ( 'NONE',  ( -1.000000000000000000, -0.000000000000000000, -0.000000000000000000 ) ) ;
#710 = ADVANCED_FACE ( 'NONE', ( #1827 ), #5856, .F. ) ;
#711 = CARTESIAN_POINT ( 'NONE',  ( -76.15625000204838102, 80.81189881250000440, -1.580522963032174394E-15 ) ) ;
#712 = LINE ( 'NONE', #6193, #3438 ) ;
#713 = EDGE_LOOP ( 'NONE', ( #11377, #7076, #6758, #8092 ) ) ;
#714 = DIRECTION ( 'NONE',  ( 0.000000000000000000, 0.000000000000000000, 1.000000000000000000 ) ) ;
#715 = EDGE_LOOP ( 'NONE', ( #11097, #2302, #10666, #3336 ) ) ;
#716 = CARTESIAN_POINT ( 'NONE',  ( 23.71418293028490609, 78.65541738657648807, 8.238313537303401546 ) ) ;
#717 = CARTESIAN_POINT ( 'NONE',  ( -37.91582326205369213, 52.94892034820053084, -6.747764776534440401 ) ) ;
#718 = DIRECTION ( 'NONE',  ( 0.000000000000000000, 1.000000000000000000, 0.000000000000000000 ) ) ;
#719 = CARTESIAN_POINT ( 'NONE',  ( -3.000000000000000000, 0.000000000000000000, -3.482085714285714229 ) ) ;
#720 = AXIS2_PLACEMENT_3D ( 'NONE', #11548, #3350, #6967 ) ;
#721 = DIRECTION ( 'NONE',  ( -1.000000000000000000, -0.000000000000000000, -0.000000000000000000 ) ) ;
#722 = CARTESIAN_POINT ( 'NONE',  ( -74.65625000204838102, 80.81189881250000440, -1.580522963032174394E-15 ) ) ;
#723 = VERTEX_POINT ( 'NONE', #1773 ) ;
#724 = DIRECTION ( 'NONE',  ( -0.000000000000000000, -0.000000000000000000, -1.000000000000000000 ) ) ;
#725 = CARTESIAN_POINT ( 'NONE',  ( -78.50000000204840944, 44.30836144126053000, 25.81189881250000795 ) ) ;
#726 = EDGE_CURVE ( 'NONE', #10529, #7325, #4652, .T. ) ;
#727 = DIRECTION ( 'NONE',  ( -1.000000000000000000, -0.000000000000000000, -0.000000000000000000 ) ) ;
#728 = CARTESIAN_POINT ( 'NONE',  ( -76.62500000409677625, 55.00000000000000000, 24.99999999999999645 ) ) ;
#729 = CARTESIAN_POINT ( 'NONE',  ( 9.097072198540729460, 54.98136927407220753, 0.006368393940946715480 ) ) ;
#730 = CARTESIAN_POINT ( 'NONE',  ( -75.00000000000001421, 29.55542218757419803, 0.4186910811744771199 ) ) ;
#731 = EDGE_LOOP ( 'NONE', ( #2625, #3077 ) ) ;
#732 = CARTESIAN_POINT ( 'NONE',  ( -10.79095582353838090, 59.95900821267746750, -0.6598374012892626039 ) ) ;
#733 = EDGE_CURVE ( 'NONE', #9917, #5658, #853, .T. ) ;
#734 = PRESENTATION_LAYER_ASSIGNMENT (  '', '', ( #6123 ) ) ;
#735 = DIRECTION ( 'NONE',  ( -0.000000000000000000, -0.000000000000000000, 1.000000000000000000 ) ) ;
#736 = ORIENTED_EDGE ( 'NONE', *, *, #5482, .T. ) ;
#737 = CARTESIAN_POINT ( 'NONE',  ( -31.45202553487676411, 34.20668501241195969, 3.085052028771560373 ) ) ;
#738 = CARTESIAN_POINT ( 'NONE',  ( -77.46875000204839523, 73.25176868561975141, 18.25176868561974075 ) ) ;
#739 = CONICAL_SURFACE ( 'NONE', #2475, 3.000000000000000000, 0.9599310885968912466 ) ;
#740 = EDGE_LOOP ( 'NONE', ( #1211, #3386, #10270, #4950, #9708, #4672 ) ) ;
#741 = EDGE_CURVE ( 'NONE', #11218, #4164, #289, .T. ) ;
#742 = CARTESIAN_POINT ( 'NONE',  ( -72.40625000204838102, 29.18810118750000271, 4.741568889096522788E-15 ) ) ;
#743 = CARTESIAN_POINT ( 'NONE',  ( 14.85570562722353749, 52.25434861561973321, 21.02374011750137939 ) ) ;
#744 = ORIENTED_EDGE ( 'NONE', *, *, #1054, .T. ) ;
#745 = CARTESIAN_POINT ( 'NONE',  ( 52.99999999999999289, 97.00000000000000000, -9.797174393178809880E-16 ) ) ;
#746 = CARTESIAN_POINT ( 'NONE',  ( 7.876834456762007441, 50.04083008229487461, 0.6585545532920904499 ) ) ;
#747 = CARTESIAN_POINT ( 'NONE',  ( 11.09270675091795511, 55.00778140979137021, -0.01448337108733858611 ) ) ;
#748 = VECTOR ( 'NONE', #2550, 1000.000000000000000 ) ;
#749 = ORIENTED_EDGE ( 'NONE', *, *, #5956, .F. ) ;
#750 = CARTESIAN_POINT ( 'NONE',  ( 4.214641129381988094, 34.60917520197180153, -5.106920541952282733 ) ) ;
#751 = CARTESIAN_POINT ( 'NONE',  ( -4.188986194789085182, 52.25407379690145859, -20.98118322582191908 ) ) ;
#752 = CARTESIAN_POINT ( 'NONE',  ( 0.000000000000000000, 0.000000000000000000, 0.000000000000000000 ) ) ;
#753 = DIRECTION ( 'NONE',  ( -1.000000000000000000, -0.000000000000000000, -0.000000000000000000 ) ) ;
#754 = DIRECTION ( 'NONE',  ( -1.000000000000000000, -0.000000000000000000, -0.000000000000000000 ) ) ;
#755 = EDGE_LOOP ( 'NONE', ( #5969, #1527, #204, #6990 ) ) ;
#756 = CARTESIAN_POINT ( 'NONE',  ( -76.43750000000005684, 72.67766952966361771, 17.67766952966361771 ) ) ;
#757 = DIRECTION ( 'NONE',  ( 0.000000000000000000, 0.000000000000000000, -1.000000000000000000 ) ) ;
#758 = DIRECTION ( 'NONE',  ( 1.000000000000000000, 0.000000000000000000, 0.000000000000000000 ) ) ;
#759 = CARTESIAN_POINT ( 'NONE',  ( -64.47562408583945626, 38.19583575827792288, 12.92744520505189953 ) ) ;
#760 = VERTEX_POINT ( 'NONE', #10090 ) ;
#761 = DIRECTION ( 'NONE',  ( 0.000000000000000000, 0.000000000000000000, 1.000000000000000000 ) ) ;
#762 = CARTESIAN_POINT ( 'NONE',  ( -78.00000000000002842, 50.75735931288069480, 2.742644059037076865 ) ) ;
#763 = B_SPLINE_CURVE_WITH_KNOTS ( 'NONE', 3,
 ( #2945, #11252, #6612, #5710, #177, #2885, #3718, #10057, #10117, #6673, #7383, #6488, #10302, #1917, #5585, #3779, #4804, #9408, #8461, #10239, #1201, #8516, #297, #9170, #4743, #9347, #4678, #1016, #7622, #1855, #6554, #1135, #8329, #7448, #10183, #239, #9282, #1319, #3124, #9702 ),
 .UNSPECIFIED., .F., .F.,
 ( 4, 2, 2, 2, 2, 2, 2, 2, 2, 2, 2, 2, 2, 2, 2, 2, 2, 2, 2, 4 ),
 ( 2.472710646779110686E-15, 0.003130555644250782206, 0.006261111288499070747, 0.009391666932747358421, 0.01095694475487150529, 0.01252222257699565390, 0.01565277822124398407, 0.01721805604336814829, 0.01878333386549230904, 0.02504444515398900756, 0.02660972297611319259, 0.02817500079823737763, 0.03130555644248574770, 0.03443611208673411084, 0.03600138990885830281, 0.03756666773098249479, 0.04382777901947923493, 0.04539305684160341997, 0.04695833466372760501, 0.05008889030797599590 ),
 .UNSPECIFIED. ) ;
#764 = ORIENTED_EDGE ( 'NONE', *, *, #8944, .F. ) ;
#765 = CARTESIAN_POINT ( 'NONE',  ( 0.000000000000000000, 0.000000000000000000, -3.131981945180866589 ) ) ;
#766 = VECTOR ( 'NONE', #5661, 1000.000000000000000 ) ;
#767 = CARTESIAN_POINT ( 'NONE',  ( -67.17448730496187181, 36.66801277209461318, 10.55271442276269944 ) ) ;
#768 = CARTESIAN_POINT ( 'NONE',  ( -76.53125000204838102, 55.00000000000000000, -25.81189881249999729 ) ) ;
#769 = CARTESIAN_POINT ( 'NONE',  ( -74.84375000204839523, 73.25176868561975141, -18.25176868561974430 ) ) ;
#770 = ORIENTED_EDGE ( 'NONE', *, *, #9291, .F. ) ;
#771 = FACE_OUTER_BOUND ( 'NONE', #5097, .T. ) ;
#772 = AXIS2_PLACEMENT_3D ( 'NONE', #6466, #10095, #5562 ) ;
#773 = ORIENTED_EDGE ( 'NONE', *, *, #9797, .T. ) ;
#774 = CARTESIAN_POINT ( 'NONE',  ( -2.626967639481237349, 55.33059824256177706, -5.000002997081709921 ) ) ;
#775 = CARTESIAN_POINT ( 'NONE',  ( 21.46051530992876977, 66.17699122582456539, 8.587284035366270274 ) ) ;
#776 = EDGE_CURVE ( 'NONE', #2110, #3954, #9275, .T. ) ;
#777 = DIRECTION ( 'NONE',  ( -0.000000000000000000, -1.000000000000000000, -0.000000000000000000 ) ) ;
#778 = CARTESIAN_POINT ( 'NONE',  ( 1.837682338809236926, 65.11633786365413812, -19.53622259640674130 ) ) ;
#779 = AXIS2_PLACEMENT_3D ( 'NONE', #3024, #6692, #198 ) ;
#780 = VECTOR ( 'NONE', #11369, 1000.000000000000000 ) ;
#781 = CARTESIAN_POINT ( 'NONE',  ( -80.00000000000002842, 42.27207793864211283, 4.242644059037075976 ) ) ;
#782 = ORIENTED_EDGE ( 'NONE', *, *, #7210, .T. ) ;
#783 =( NAMED_UNIT ( * ) PLANE_ANGLE_UNIT ( ) SI_UNIT ( $, .RADIAN. ) );
#784 = CARTESIAN_POINT ( 'NONE',  ( -76.06250000204840944, 80.81189881250001861, -10.69163855873949132 ) ) ;
#785 = ADVANCED_FACE ( 'NONE', ( #1357 ), #392, .F. ) ;
#786 = CARTESIAN_POINT ( 'NONE',  ( -2.500000000000000000, 3.061616997868383141E-16, -3.131981945180866589 ) ) ;
#787 = CARTESIAN_POINT ( 'NONE',  ( 39.99999999999999289, 55.00000000000000000, -24.99999999999999645 ) ) ;
#788 = CARTESIAN_POINT ( 'NONE',  ( -43.43046782438146636, 54.98524932194441561, 0.01300693185584521350 ) ) ;
#789 = CIRCLE ( 'NONE', #978, 2.500000000000000000 ) ;
#790 = CARTESIAN_POINT ( 'NONE',  ( -75.00000000000000000, 34.71505921034813724, 14.90932262158721500 ) ) ;
#791 = ORIENTED_EDGE ( 'NONE', *, *, #3827, .T. ) ;
#792 = CARTESIAN_POINT ( 'NONE',  ( -21.29436769408802377, 54.66877947394643655, 4.999995929924349269 ) ) ;
#793 = CARTESIAN_POINT ( 'NONE',  ( -68.81799204399976588, 34.52608862562686909, 5.501299279293338174 ) ) ;
#794 = ORIENTED_EDGE ( 'NONE', *, *, #4701, .F. ) ;
#795 = CARTESIAN_POINT ( 'NONE',  ( -43.11869212536358020, 60.10704077131471479, -20.39111636944713624 ) ) ;
#796 = FACE_OUTER_BOUND ( 'NONE', #4135, .T. ) ;
#797 = EDGE_CURVE ( 'NONE', #10685, #2528, #2250, .T. ) ;
#798 = EDGE_CURVE ( 'NONE', #1970, #8495, #11569, .T. ) ;
#799 = EDGE_CURVE ( 'NONE', #1715, #10833, #3542, .T. ) ;
#800 = ORIENTED_EDGE ( 'NONE', *, *, #878, .F. ) ;
#801 = CARTESIAN_POINT ( 'NONE',  ( -72.68750000204839523, 44.30836144126053000, 25.81189881250000795 ) ) ;
#802 = CARTESIAN_POINT ( 'NONE',  ( 0.8557374297261139962, 42.07536394375442512, -16.80742094040031631 ) ) ;
#803 = ADVANCED_FACE ( 'NONE', ( #4958 ), #1174, .F. ) ;
#804 = EDGE_CURVE ( 'NONE', #19, #11526, #11182, .T. ) ;
#805 = DIRECTION ( 'NONE',  ( -1.000000000000000000, -0.000000000000000000, -0.000000000000000000 ) ) ;
#806 = CARTESIAN_POINT ( 'NONE',  ( -9.204882831600160742, 55.00123686646767851, -0.002328140736296190928 ) ) ;
#807 = ORIENTED_EDGE ( 'NONE', *, *, #3450, .T. ) ;
#808 = ADVANCED_FACE ( 'NONE', ( #9564 ), #5862, .T. ) ;
#809 = CARTESIAN_POINT ( 'NONE',  ( 11.85573742417284748, 44.41863851231033067, 18.37121583117139778 ) ) ;
#810 = CARTESIAN_POINT ( 'NONE',  ( -7.929357056070021947, 64.91238717040420170, -18.54984206437098493 ) ) ;
#811 = CARTESIAN_POINT ( 'NONE',  ( 4.999999999999998224, -2.886751345948137981, -5.653418012614792154 ) ) ;
#812 = CARTESIAN_POINT ( 'NONE',  ( -75.50000000000001421, 54.99999999999944578, -24.99999999999999645 ) ) ;
#813 = CARTESIAN_POINT ( 'NONE',  ( 0.000000000000000000, 0.000000000000000000, 0.000000000000000000 ) ) ;
#814 = EDGE_LOOP ( 'NONE', ( #11632, #7183, #5168, #5466 ) ) ;
#815 = CARTESIAN_POINT ( 'NONE',  ( -77.00000000000000000, 55.00000000000000000, -24.99999999999999645 ) ) ;
#816 = DIRECTION ( 'NONE',  ( -1.000000000000000000, 0.000000000000000000, -0.000000000000000000 ) ) ;
#817 = FACE_OUTER_BOUND ( 'NONE', #7666, .T. ) ;
#818 = VERTEX_POINT ( 'NONE', #2135 ) ;
#819 = DIRECTION ( 'NONE',  ( 1.000000000000000000, 6.033820786006286457E-17, -0.000000000000000000 ) ) ;
#820 = CARTESIAN_POINT ( 'NONE',  ( -60.98114229612854587, 55.65873833719333419, 4.967062080433862548 ) ) ;
#821 = EDGE_LOOP ( 'NONE', ( #3246, #9640, #10740, #10037 ) ) ;
#822 = DIRECTION ( 'NONE',  ( 0.000000000000000000, 0.000000000000000000, 1.000000000000000000 ) ) ;
#823 = CARTESIAN_POINT ( 'NONE',  ( -83.00000000000000000, 55.00000000000000000, 20.00000000000000355 ) ) ;
#824 = CARTESIAN_POINT ( 'NONE',  ( -71.95822497812569907, 74.53807824654330716, 16.15905817987090032 ) ) ;
#825 = CARTESIAN_POINT ( 'NONE',  ( 0.000000000000000000, 0.000000000000000000, -1.753742857142857048 ) ) ;
#826 = ORIENTED_EDGE ( 'NONE', *, *, #2571, .T. ) ;
#827 = CARTESIAN_POINT ( 'NONE',  ( -76.81250000204839523, 29.18810118750000981, 10.69163855873950020 ) ) ;
#828 = ORIENTED_EDGE ( 'NONE', *, *, #4635, .T. ) ;
#829 = CARTESIAN_POINT ( 'NONE',  ( 5.447911505823581635, 66.41754438690165330, 22.24099615069902569 ) ) ;
#830 = CARTESIAN_POINT ( 'NONE',  ( -6.455306493259947764, 63.34608869971732048, -11.25480877436020855 ) ) ;
#831 = AXIS2_PLACEMENT_3D ( 'NONE', #7959, #7072, #7186 ) ;
#832 = CARTESIAN_POINT ( 'NONE',  ( -76.53125000204839523, 36.74823131438024859, -18.25176868561973720 ) ) ;
#833 = CARTESIAN_POINT ( 'NONE',  ( -78.00000000000001421, 42.27207793864211283, -12.72791868944003824 ) ) ;
#834 = CARTESIAN_POINT ( 'NONE',  ( 4.999999999999998224, -2.886751345948137981, -5.653418012614792154 ) ) ;
#835 = B_SPLINE_CURVE_WITH_KNOTS ( 'NONE', 3,
 ( #2892, #1982, #4749, #2043, #8400, #3851, #7516, #2952, #9062, #6740, #4029, #2165, #11199, #9414, #8645, #2105, #7686, #5895, #6859, #7628, #3970, #11321, #8701, #5053, #5835, #9536, #3245, #11259, #9475, #1263, #4141, #4085, #3070, #4932, #7803, #5778, #6796, #1392 ),
 .UNSPECIFIED., .F., .F.,
 ( 4, 2, 2, 2, 2, 2, 2, 2, 2, 2, 2, 2, 2, 2, 2, 2, 2, 2, 4 ),
 ( 0.07285479446859771668, 0.07361368492618262926, 0.07437257538376754185, 0.07589035629893736701, 0.07740813721410717829, 0.07892591812927700345, 0.08044369904444681474, 0.08196147995961662602, 0.08347926087478645119, 0.08499704178995626247, 0.08575593224754117505, 0.08651482270512608763, 0.08803260362029592667, 0.08955038453546575183, 0.09106816545063559087, 0.09258594636580541604, 0.09410372728097524120, 0.09562150819614508024, 0.09713928911131490540 ),
 .UNSPECIFIED. ) ;
#836 = EDGE_LOOP ( 'NONE', ( #265, #11815, #613, #5640, #1780, #6974 ) ) ;
#837 = FILL_AREA_STYLE ('',( #4508 ) ) ;
#838 = CARTESIAN_POINT ( 'NONE',  ( -75.59375000409679046, 80.00000000000001421, -10.35533905932737753 ) ) ;
#839 = EDGE_CURVE ( 'NONE', #5641, #4778, #6767, .T. ) ;
#840 = DIRECTION ( 'NONE',  ( -1.000000000000000000, -6.033820786006286457E-17, -0.000000000000000000 ) ) ;
#841 = DIRECTION ( 'NONE',  ( -1.000000000000000000, -0.000000000000000000, -0.000000000000000000 ) ) ;
#842 = CARTESIAN_POINT ( 'NONE',  ( -38.17020195889585921, 54.99973427304116314, 0.005832240597639265153 ) ) ;
#843 = CONTEXT_DEPENDENT_SHAPE_REPRESENTATION ( #9447, #10164 ) ;
#844 =( GEOMETRIC_REPRESENTATION_CONTEXT ( 3 ) GLOBAL_UNCERTAINTY_ASSIGNED_CONTEXT ( ( #5921 ) ) GLOBAL_UNIT_ASSIGNED_CONTEXT ( ( #5850, #10497, #257 ) ) REPRESENTATION_CONTEXT ( 'NONE', 'WORKASPACE' ) );
#845 = CARTESIAN_POINT ( 'NONE',  ( -21.70513237093992132, 76.99208176644971502, 0.6955368305833549147 ) ) ;
#846 = CARTESIAN_POINT ( 'NONE',  ( -20.12390779004163477, 55.65879866787057750, 4.959133026351390860 ) ) ;
#847 = VERTEX_POINT ( 'NONE', #8429 ) ;
#848 = CARTESIAN_POINT ( 'NONE',  ( -63.32723919479404628, 46.95276866351182576, 19.42062151208882170 ) ) ;
#849 = VERTEX_POINT ( 'NONE', #7717 ) ;
#850 = CARTESIAN_POINT ( 'NONE',  ( -13.52239577877046095, 75.98118489547775312, -2.745668029642679642 ) ) ;
#851 = CARTESIAN_POINT ( 'NONE',  ( -72.12500000204839523, 44.30836144126050158, -25.81189881249999374 ) ) ;
#852 = PRODUCT_DEFINITION_FORMATION_WITH_SPECIFIED_SOURCE ( 'ANY', '', #3760, .NOT_KNOWN. ) ;
#853 = CIRCLE ( 'NONE', #2783, 4.171999999999999709 ) ;
#854 = ORIENTED_EDGE ( 'NONE', *, *, #8075, .F. ) ;
#855 = CARTESIAN_POINT ( 'NONE',  ( -75.03125000204838102, 55.00000000000000000, -25.81189881249999729 ) ) ;
#856 = CARTESIAN_POINT ( 'NONE',  ( -29.26269115883859939, 34.87241548204915631, 6.108265559058850158 ) ) ;
#857 = SHAPE_REPRESENTATION_RELATIONSHIP ( 'NONE' , 'NONE' ,  #3715, #1113 ) ;
#858 = ORIENTED_EDGE ( 'NONE', *, *, #6456, .F. ) ;
#859 = DIRECTION ( 'NONE',  ( -0.000000000000000000, 1.000000000000000000, 0.000000000000000000 ) ) ;
#860 = CARTESIAN_POINT ( 'NONE',  ( -60.50017553191300834, 56.37004246370271687, 6.895233585243415675 ) ) ;
#861 = CIRCLE ( 'NONE', #9487, 1.500000000000001332 ) ;
#862 = ORIENTED_EDGE ( 'NONE', *, *, #587, .F. ) ;
#863 = CARTESIAN_POINT ( 'NONE',  ( 20.47769554116023372, 71.77531707407277395, 12.89192088424961824 ) ) ;
#864 = CARTESIAN_POINT ( 'NONE',  ( -8.785358865379802040, 67.52185545713140868, -16.88477868139494831 ) ) ;
#865 = FACE_OUTER_BOUND ( 'NONE', #7245, .T. ) ;
#866 = CYLINDRICAL_SURFACE ( 'NONE', #6599, 1.499999999999999556 ) ;
#867 = CARTESIAN_POINT ( 'NONE',  ( 0.000000000000000000, 0.000000000000000000, 0.000000000000000000 ) ) ;
#868 = CARTESIAN_POINT ( 'NONE',  ( -2.925285743277529438, -4.084588180558409221, -6.089444439476603854 ) ) ;
#869 = EDGE_CURVE ( 'NONE', #8948, #11420, #9501, .T. ) ;
#870 = ORIENTED_EDGE ( 'NONE', *, *, #7718, .F. ) ;
#871 = CARTESIAN_POINT ( 'NONE',  ( 47.00000000000000000, 55.00000000000000000, 0.000000000000000000 ) ) ;
#872 = CARTESIAN_POINT ( 'NONE',  ( -13.75936034494452542, 55.01575878706701417, -0.004732648836832428763 ) ) ;
#873 = CARTESIAN_POINT ( 'NONE',  ( -55.12858368788357666, 57.50315721827126936, 4.331434029952367482 ) ) ;
#874 = VECTOR ( 'NONE', #8482, 1000.000000000000000 ) ;
#875 = CARTESIAN_POINT ( 'NONE',  ( 34.00000000000000000, 55.00000000000000000, 0.000000000000000000 ) ) ;
#876 = AXIS2_PLACEMENT_3D ( 'NONE', #2832, #11141, #188 ) ;
#877 = CYLINDRICAL_SURFACE ( 'NONE', #4723, 1.500000000000000000 ) ;
#878 = EDGE_CURVE ( 'NONE', #7673, #884, #5469, .T. ) ;
#879 = VERTEX_POINT ( 'NONE', #5025 ) ;
#880 = CARTESIAN_POINT ( 'NONE',  ( -80.00000000000001421, 67.72792206135787296, -11.22791868944004534 ) ) ;
#881 = DIRECTION ( 'NONE',  ( -1.000000000000000000, -0.000000000000000000, -0.000000000000000000 ) ) ;
#882 = CARTESIAN_POINT ( 'NONE',  ( 19.12485590497331245, 59.33891611993333726, 2.506220315686558564 ) ) ;
#883 = CARTESIAN_POINT ( 'NONE',  ( -72.96875000204838102, 73.25176868561975141, 18.25176868561974075 ) ) ;
#884 = VERTEX_POINT ( 'NONE', #10274 ) ;
#885 = VECTOR ( 'NONE', #3491, 1000.000000000000000 ) ;
#886 = CARTESIAN_POINT ( 'NONE',  ( -75.03125000204839523, 36.74823131438024859, -18.25176868561973720 ) ) ;
#887 = ORIENTED_EDGE ( 'NONE', *, *, #6671, .T. ) ;
#888 = CARTESIAN_POINT ( 'NONE',  ( 18.41792582001188805, 74.34136002823915135, 15.84364092613776975 ) ) ;
#889 = VECTOR ( 'NONE', #6874, 1000.000000000000000 ) ;
#890 = CARTESIAN_POINT ( 'NONE',  ( -3.262052055525263228, 56.37336850891590956, -14.01842231928934090 ) ) ;
#891 = CARTESIAN_POINT ( 'NONE',  ( -76.62500000204838102, 29.18810118750000626, -10.69163855873949132 ) ) ;
#892 = CARTESIAN_POINT ( 'NONE',  ( -79.15625000000001421, 44.64466094067263668, 24.99999999999997513 ) ) ;
#893 = FACE_OUTER_BOUND ( 'NONE', #5900, .T. ) ;
#894 = VECTOR ( 'NONE', #2900, 1000.000000000000000 ) ;
#895 = AXIS2_PLACEMENT_3D ( 'NONE', #11702, #4576, #8117 ) ;
#896 = VERTEX_POINT ( 'NONE', #10448 ) ;
#897 = CARTESIAN_POINT ( 'NONE',  ( -76.62500000409677625, 55.00000000000000000, 24.99999999999999645 ) ) ;
#898 = CARTESIAN_POINT ( 'NONE',  ( -75.50000000409677625, 80.00000000000000000, -1.530808498934191324E-15 ) ) ;
#899 = EDGE_CURVE ( 'NONE', #3592, #7749, #2919, .T. ) ;
#900 = DIRECTION ( 'NONE',  ( 1.000000000000000000, 0.000000000000000000, 0.000000000000000000 ) ) ;
#901 = CARTESIAN_POINT ( 'NONE',  ( -31.76380171923032947, 55.01766230220479059, 0.008650971149387511397 ) ) ;
#902 = CONTEXT_DEPENDENT_SHAPE_REPRESENTATION ( #11428, #1079 ) ;
#903 = VECTOR ( 'NONE', #3004, 1000.000000000000000 ) ;
#904 = CARTESIAN_POINT ( 'NONE',  ( -18.37414261478594213, 74.25662752951258483, -10.65766454279107478 ) ) ;
#905 = LINE ( 'NONE', #4465, #8956 ) ;
#906 = ORIENTED_EDGE ( 'NONE', *, *, #8266, .F. ) ;
#907 = PLANE ( 'NONE',  #10710 ) ;
#908 = ORIENTED_EDGE ( 'NONE', *, *, #2554, .T. ) ;
#909 = CARTESIAN_POINT ( 'NONE',  ( -15.14429485721040614, 76.01882847486140804, 2.745652427074330326 ) ) ;
#910 = CARTESIAN_POINT ( 'NONE',  ( -71.84375000204838102, 73.25176868561975141, -18.25176868561974430 ) ) ;
#911 = VERTEX_POINT ( 'NONE', #7767 ) ;
#912 = MANIFOLD_SOLID_BREP ( 'Cavity1', #11314 ) ;
#913 = EDGE_CURVE ( 'NONE', #1407, #8886, #6011, .T. ) ;
#914 = CARTESIAN_POINT ( 'NONE',  ( -74.18750000204838102, 44.30836144126053000, 25.81189881250000795 ) ) ;
#915 = CARTESIAN_POINT ( 'NONE',  ( 2.274842917244503937, 38.70728229458904934, -13.38060881307704975 ) ) ;
#916 =( NAMED_UNIT ( * ) SI_UNIT ( $, .STERADIAN. ) SOLID_ANGLE_UNIT ( ) );
#917 = AXIS2_PLACEMENT_3D ( 'NONE', #6828, #10454, #10804 ) ;
#918 = EDGE_LOOP ( 'NONE', ( #7409, #3396 ) ) ;
#919 = B_SPLINE_CURVE_WITH_KNOTS ( 'NONE', 3,
 ( #8394, #9528, #1074, #10301 ),
 .UNSPECIFIED., .F., .F.,
 ( 4, 4 ),
 ( 0.000000000000000000, 1.000000000000000000 ),
 .UNSPECIFIED. ) ;
#920 = FACE_OUTER_BOUND ( 'NONE', #10715, .T. ) ;
#921 = CARTESIAN_POINT ( 'NONE',  ( -64.29142959965328430, 52.00076317697213568, 6.340235024524601748 ) ) ;
#922 = ORIENTED_EDGE ( 'NONE', *, *, #35, .F. ) ;
#923 = CARTESIAN_POINT ( 'NONE',  ( -41.59602423483332956, 57.05917253807995593, -20.93237218927098198 ) ) ;
#924 = AXIS2_PLACEMENT_3D ( 'NONE', #3401, #7187, #2623 ) ;
#925 = CARTESIAN_POINT ( 'NONE',  ( -7.337209909475700620, 63.04728967918421745, -19.42673836724018699 ) ) ;
#926 = CARTESIAN_POINT ( 'NONE',  ( -5.000000000000000000, -2.886751345948134428, -0.4465819873852071575 ) ) ;
#927 = DIRECTION ( 'NONE',  ( 6.033820786006286457E-17, -1.000000000000000000, 0.000000000000000000 ) ) ;
#928 = VECTOR ( 'NONE', #3584, 1000.000000000000000 ) ;
#929 = DIRECTION ( 'NONE',  ( 0.000000000000000000, 0.000000000000000000, 1.000000000000000000 ) ) ;
#930 = CARTESIAN_POINT ( 'NONE',  ( -78.00000000000001421, 63.48528137423857487, 6.985284746156351865 ) ) ;
#931 = EDGE_CURVE ( 'NONE', #3874, #11822, #10991, .T. ) ;
#932 = VERTEX_POINT ( 'NONE', #10728 ) ;
#933 = CARTESIAN_POINT ( 'NONE',  ( 5.000000000000000000, 2.886751345948124214, -6.099999999999999645 ) ) ;
#934 = CARTESIAN_POINT ( 'NONE',  ( -31.66451884688278184, 54.99809435283415837, 0.0005903141131624571472 ) ) ;
#935 = CARTESIAN_POINT ( 'NONE',  ( -53.18446182085578045, 58.76752042146932098, 3.303451655433074396 ) ) ;
#936 = AXIS2_PLACEMENT_3D ( 'NONE', #10985, #6463, #1890 ) ;
#937 = CARTESIAN_POINT ( 'NONE',  ( -74.93750000000007105, 72.67766952966361771, 17.67766952966360350 ) ) ;
#938 = AXIS2_PLACEMENT_3D ( 'NONE', #11200, #1023, #6006 ) ;
#939 = CARTESIAN_POINT ( 'NONE',  ( -77.37500000409677625, 55.00000000000000000, -24.99999999999999645 ) ) ;
#940 = EDGE_LOOP ( 'NONE', ( #4887, #4146, #3980, #10315 ) ) ;
#941 = CARTESIAN_POINT ( 'NONE',  ( -9.391823749396904120, 73.59702374900430755, -9.931971109272440756 ) ) ;
#942 = CARTESIAN_POINT ( 'NONE',  ( 2.400054171417768487E-15, 64.99605696851786263, -19.59792961213366169 ) ) ;
#943 = CARTESIAN_POINT ( 'NONE',  ( 17.18511958428734232, 58.30390285059421984, 3.767129572935171034 ) ) ;
#944 = CARTESIAN_POINT ( 'NONE',  ( -73.34375000204839523, 73.25176868561975141, -18.25176868561974430 ) ) ;
#945 = CARTESIAN_POINT ( 'NONE',  ( -76.71875000204839523, 36.74823131438024859, -18.25176868561973720 ) ) ;
#946 = EDGE_CURVE ( 'NONE', #7264, #10278, #57, .T. ) ;
#947 = ORIENTED_EDGE ( 'NONE', *, *, #7700, .T. ) ;
#948 = ADVANCED_FACE ( 'NONE', ( #3549 ), #2653, .T. ) ;
#949 = CARTESIAN_POINT ( 'NONE',  ( -78.68750000204839523, 65.69163855873949842, 25.81189881250000440 ) ) ;
#950 = ORIENTED_EDGE ( 'NONE', *, *, #804, .T. ) ;
#951 = CARTESIAN_POINT ( 'NONE',  ( -5.349432795815419084, 57.50648965827332404, -4.338654380549343159 ) ) ;
#952 = CARTESIAN_POINT ( 'NONE',  ( -28.03633875861160263, 42.33641998042576660, 5.989639417439852842 ) ) ;
#953 = CARTESIAN_POINT ( 'NONE',  ( -75.00000000000000000, 55.00000000000000000, 29.00000000000000355 ) ) ;
#954 = FACE_OUTER_BOUND ( 'NONE', #6624, .T. ) ;
#955 = AXIS2_PLACEMENT_3D ( 'NONE', #8147, #9335, #10229 ) ;
#956 = EDGE_CURVE ( 'NONE', #9492, #656, #6378, .T. ) ;
#957 = ADVANCED_FACE ( 'NONE', ( #1749 ), #7221, .F. ) ;
#958 = DIRECTION ( 'NONE',  ( 0.000000000000000000, 0.000000000000000000, -1.000000000000000000 ) ) ;
#959 = EDGE_LOOP ( 'NONE', ( #4734, #11437 ) ) ;
#960 = EDGE_CURVE ( 'NONE', #2363, #8766, #6620, .T. ) ;
#961 = VECTOR ( 'NONE', #1461, 1000.000000000000000 ) ;
#962 = CARTESIAN_POINT ( 'NONE',  ( -79.43750000000001421, 72.67766952966368876, 17.67766952966368521 ) ) ;
#963 = CARTESIAN_POINT ( 'NONE',  ( -73.25000000204839523, 65.69163855873948421, -25.81189881250000440 ) ) ;
#964 = CARTESIAN_POINT ( 'NONE',  ( 5.000000000000000888, 0.000000000000000000, -6.099999999999999645 ) ) ;
#965 = AXIS2_PLACEMENT_3D ( 'NONE', #5635, #6779, #4790 ) ;
#966 = CARTESIAN_POINT ( 'NONE',  ( -44.75936011935566228, 55.01969457619907899, -0.01734821724329012674 ) ) ;
#967 = APPLICATION_PROTOCOL_DEFINITION ( 'draft international standard', 'automotive_design', 1998, #4096 ) ;
#968 = DIRECTION ( 'NONE',  ( -1.000000000000000000, -0.000000000000000000, -0.000000000000000000 ) ) ;
#969 = AXIS2_PLACEMENT_3D ( 'NONE', #3189, #10486, #2290 ) ;
#970 = CARTESIAN_POINT ( 'NONE',  ( -20.71005862496660654, 55.16551809362240988, 5.000002034471375367 ) ) ;
#971 = ORIENTED_EDGE ( 'NONE', *, *, #602, .T. ) ;
#972 = DIRECTION ( 'NONE',  ( -0.000000000000000000, -0.000000000000000000, -1.000000000000000000 ) ) ;
#973 = CARTESIAN_POINT ( 'NONE',  ( 2.500000000000000000, 0.000000000000000000, -3.996153373752295401 ) ) ;
#974 = ORIENTED_EDGE ( 'NONE', *, *, #11026, .T. ) ;
#975 = CARTESIAN_POINT ( 'NONE',  ( 10.52240409369262153, 44.41989175727180594, 18.36819097564579195 ) ) ;
#976 = CARTESIAN_POINT ( 'NONE',  ( -78.21875000204839523, 29.18810118750000271, 4.741568889096522788E-15 ) ) ;
#977 = CONICAL_SURFACE ( 'NONE', #8454, 2.500000000000000000, 0.9599310885968755924 ) ;
#978 = AXIS2_PLACEMENT_3D ( 'NONE', #596, #3239, #8754 ) ;
#979 = ORIENTED_EDGE ( 'NONE', *, *, #1682, .T. ) ;
#980 = MANIFOLD_SOLID_BREP ( 'Cavity1', #6172 ) ;
#981 = CARTESIAN_POINT ( 'NONE',  ( -72.31250000204839523, 29.18810118750000626, -10.69163855873949309 ) ) ;
#982 = CARTESIAN_POINT ( 'NONE',  ( -23.18906244097991021, 49.50939288222085821, 20.43027456479002879 ) ) ;
#983 =( NAMED_UNIT ( * ) SI_UNIT ( $, .STERADIAN. ) SOLID_ANGLE_UNIT ( ) );
#984 = CARTESIAN_POINT ( 'NONE',  ( -60.45014771802851072, 49.89223742090062075, 20.38901927491476584 ) ) ;
#985 = ORIENTED_EDGE ( 'NONE', *, *, #11608, .F. ) ;
#986 = CARTESIAN_POINT ( 'NONE',  ( -8.287358458837889685, 57.06376126929644954, -4.557158438297962633 ) ) ;
#987 = CARTESIAN_POINT ( 'NONE',  ( -1.144262565995328940, 42.07883645215377300, -16.80394782698530065 ) ) ;
#988 = EDGE_LOOP ( 'NONE', ( #8464, #10923 ) ) ;
#989 = CARTESIAN_POINT ( 'NONE',  ( -45.05849143660482525, 68.38147613270652414, -16.29358623752561641 ) ) ;
#990 = CARTESIAN_POINT ( 'NONE',  ( -11.39182375260447166, 73.60042400440836730, -9.933379572949093017 ) ) ;
#991 = CARTESIAN_POINT ( 'NONE',  ( 5.000000000000000888, -1.936377641173860908, -0.1973691732449218139 ) ) ;
#992 = LINE ( 'NONE', #1888, #5063 ) ;
#993 = CARTESIAN_POINT ( 'NONE',  ( 0.000000000000000000, 0.000000000000000000, -4.696360911962001339 ) ) ;
#994 = DIRECTION ( 'NONE',  ( -1.000000000000000000, -0.000000000000000000, -0.000000000000000000 ) ) ;
#995 = ORIENTED_EDGE ( 'NONE', *, *, #8595, .F. ) ;
#996 = EDGE_CURVE ( 'NONE', #9989, #2344, #8449, .T. ) ;
#997 = CARTESIAN_POINT ( 'NONE',  ( 34.00000000000000000, 50.00000000000001421, 6.123233995736750505E-16 ) ) ;
#998 = CARTESIAN_POINT ( 'NONE',  ( -44.79520175934491988, 54.99837535002616562, 0.003324556147400343012 ) ) ;
#999 = CARTESIAN_POINT ( 'NONE',  ( -63.28902608371529936, 51.23315991719264417, 3.304235638531133112 ) ) ;
#1000 = CARTESIAN_POINT ( 'NONE',  ( 0.000000000000000000, 0.000000000000000000, -1.403639088038009630 ) ) ;
#1001 = CARTESIAN_POINT ( 'NONE',  ( 0.000000000000000000, -17.82799999999998875, 0.000000000000000000 ) ) ;
#1002 = CARTESIAN_POINT ( 'NONE',  ( 20.77652457878251013, 61.80192317012852499, 1.825703622701588813 ) ) ;
#1003 = ORIENTED_EDGE ( 'NONE', *, *, #10279, .T. ) ;
#1004 = CARTESIAN_POINT ( 'NONE',  ( 6.636022776496402820, 34.00797225689733239, 1.031222807066483504 ) ) ;
#1005 = CARTESIAN_POINT ( 'NONE',  ( -73.06250000204842365, 80.81189881250000440, 10.69163855873948243 ) ) ;
#1006 = CARTESIAN_POINT ( 'NONE',  ( -83.00000000000000000, 55.00000000000000000, 29.00000000000000355 ) ) ;
#1007 = CARTESIAN_POINT ( 'NONE',  ( 5.126123443351389142, 50.15990383064929858, 1.295883551324225946 ) ) ;
#1008 = CARTESIAN_POINT ( 'NONE',  ( -71.48947498017410851, 75.17259594761931396, 16.68383898576512081 ) ) ;
#1009 = CARTESIAN_POINT ( 'NONE',  ( -76.43750000204838102, 65.69163855873948421, -25.81189881250000440 ) ) ;
#1010 = ORIENTED_EDGE ( 'NONE', *, *, #11325, .T. ) ;
#1011 = CARTESIAN_POINT ( 'NONE',  ( -79.15625000204839523, 73.25176868561975141, -18.25176868561974430 ) ) ;
#1012 = ORIENTED_EDGE ( 'NONE', *, *, #2580, .F. ) ;
#1013 = CARTESIAN_POINT ( 'NONE',  ( -42.63032052581742448, 60.99632860981928673, -12.67841600781651046 ) ) ;
#1014 = CARTESIAN_POINT ( 'NONE',  ( -78.96875000204839523, 80.81189881250000440, -1.580522963032174394E-15 ) ) ;
#1015 =( BOUNDED_CURVE ( )  B_SPLINE_CURVE ( 2, ( #2066, #9372, #1946, #10329, #7411, #9254, #6516, #3925, #11036 ),
 .UNSPECIFIED., .F., .T. ) 
 B_SPLINE_CURVE_WITH_KNOTS ( ( 3, 2, 2, 2, 3 ),
 ( 0.6666666666666671848, 0.6875000000000005551, 0.7083333333333339255, 0.7291666666666672958, 0.7500000000000006661 ),
 .UNSPECIFIED. ) 
 CURVE ( )  GEOMETRIC_REPRESENTATION_ITEM ( )  RATIONAL_B_SPLINE_CURVE ( ( 0.9999999999999980016, 0.9238795325112887369, 1.000000000000000000, 0.9238795325112867385, 1.000000000000000000, 0.9238795325112867385, 1.000000000000000000, 0.9238795325112842960, 1.000000000000002442 ) ) 
 REPRESENTATION_ITEM ( '' )  );
#1016 = CARTESIAN_POINT ( 'NONE',  ( -75.00000000000001421, 80.17654715216286831, -1.959916203278639024 ) ) ;
#1017 = DIRECTION ( 'NONE',  ( 0.5000000000000009992, 0.8660254037844380415, -0.000000000000000000 ) ) ;
#1018 = ORIENTED_EDGE ( 'NONE', *, *, #9096, .F. ) ;
#1019 = CARTESIAN_POINT ( 'NONE',  ( -78.96875000000000000, 30.00000000000001421, 10.35533905932739174 ) ) ;
#1020 = CARTESIAN_POINT ( 'NONE',  ( -71.56250000204838102, 80.81189881250001861, -10.69163855873949132 ) ) ;
#1021 = CARTESIAN_POINT ( 'NONE',  ( 39.99999999999999289, 55.00000000000000000, 0.000000000000000000 ) ) ;
#1022 = AXIS2_PLACEMENT_3D ( 'NONE', #7611, #11239, #3051 ) ;
#1023 = DIRECTION ( 'NONE',  ( -1.000000000000000000, -0.000000000000000000, -0.000000000000000000 ) ) ;
#1024 = EDGE_CURVE ( 'NONE', #10896, #8154, #9201, .T. ) ;
#1025 = CARTESIAN_POINT ( 'NONE',  ( -31.16317214572511674, 54.99555836494509720, -0.0001888778372106834306 ) ) ;
#1026 = CARTESIAN_POINT ( 'NONE',  ( -19.59385640182016530, 75.24237086212529846, -8.623108768566876137 ) ) ;
#1027 = CARTESIAN_POINT ( 'NONE',  ( -71.37500000409677625, 55.00000000000000000, -24.99999999999999645 ) ) ;
#1028 = ORIENTED_EDGE ( 'NONE', *, *, #10581, .T. ) ;
#1029 = CARTESIAN_POINT ( 'NONE',  ( 0.000000000000000000, 0.000000000000000000, -10.00000000000000000 ) ) ;
#1030 = EDGE_CURVE ( 'NONE', #9436, #2186, #169, .T. ) ;
#1031 = DIRECTION ( 'NONE',  ( -1.000000000000000000, -0.000000000000000000, -0.000000000000000000 ) ) ;
#1032 = EDGE_CURVE ( 'NONE', #8985, #10987, #6615, .T. ) ;
#1033 = VERTEX_POINT ( 'NONE', #6491 ) ;
#1034 = CARTESIAN_POINT ( 'NONE',  ( -62.66057256483475868, 46.95287281750281494, 19.42033498346916787 ) ) ;
#1035 = CARTESIAN_POINT ( 'NONE',  ( -77.37500000204838102, 80.81189881250001861, 10.69163855873948599 ) ) ;
#1036 = DIRECTION ( 'NONE',  ( 0.000000000000000000, 0.000000000000000000, 1.000000000000000000 ) ) ;
#1037 = CARTESIAN_POINT ( 'NONE',  ( -16.69731055678936826, 70.57278980777935828, 14.11442052818484783 ) ) ;
#1038 =( NAMED_UNIT ( * ) SI_UNIT ( $, .STERADIAN. ) SOLID_ANGLE_UNIT ( ) );
#1039 = CARTESIAN_POINT ( 'NONE',  ( -43.83980969374544401, 66.71858909844225138, -17.55257377017560216 ) ) ;
#1040 = ORIENTED_EDGE ( 'NONE', *, *, #589, .T. ) ;
#1041 = CARTESIAN_POINT ( 'NONE',  ( -72.78125000204839523, 73.25176868561975141, 18.25176868561974075 ) ) ;
#1042 = CARTESIAN_POINT ( 'NONE',  ( 1.046276059170544448, 50.44260135563150271, -2.063240075633586024 ) ) ;
#1043 = COLOUR_RGB ( '',0.8941176470588234615, 0.8941176470588234615, 0.8941176470588234615 ) ;
#1044 = CARTESIAN_POINT ( 'NONE',  ( 14.47760468889531182, 57.74566952947367326, 20.98118467575540436 ) ) ;
#1045 = PRESENTATION_LAYER_ASSIGNMENT (  '', '', ( #9094 ) ) ;
#1046 = EDGE_LOOP ( 'NONE', ( #7442, #8022 ) ) ;
#1047 = CARTESIAN_POINT ( 'NONE',  ( -42.45202546124224341, 60.10692058874730037, -20.39082473449001043 ) ) ;
#1048 = CARTESIAN_POINT ( 'NONE',  ( -50.14429338685609849, 75.46958046783008456, -5.506903914760000518 ) ) ;
#1049 = SURFACE_STYLE_FILL_AREA ( #3877 ) ;
#1050 = DIRECTION ( 'NONE',  ( -0.000000000000000000, -0.000000000000000000, -1.000000000000000000 ) ) ;
#1051 = FACE_OUTER_BOUND ( 'NONE', #755, .T. ) ;
#1052 = CYLINDRICAL_SURFACE ( 'NONE', #5002, 24.99999999999999645 ) ;
#1053 = EDGE_LOOP ( 'NONE', ( #3271, #1726, #7115, #10503 ) ) ;
#1054 = EDGE_CURVE ( 'NONE', #2054, #1879, #1860, .T. ) ;
#1055 = FACE_OUTER_BOUND ( 'NONE', #4597, .T. ) ;
#1056 = CARTESIAN_POINT ( 'NONE',  ( -16.90719202101858087, 54.98551469821890691, -0.007782449515281230322 ) ) ;
#1057 = CARTESIAN_POINT ( 'NONE',  ( -50.46075028443474508, 59.84060402248204014, 1.293943614083152394 ) ) ;
#1058 = DIRECTION ( 'NONE',  ( -1.000000000000000000, 0.000000000000000000, 0.000000000000000000 ) ) ;
#1059 = CARTESIAN_POINT ( 'NONE',  ( -56.07732272482616764, 65.82928010674932295, 8.888286616055713907 ) ) ;
#1060 = ORIENTED_EDGE ( 'NONE', *, *, #10956, .T. ) ;
#1061 = CARTESIAN_POINT ( 'NONE',  ( -78.00000000000001421, 67.72792206135787296, 4.242644059037073312 ) ) ;
#1062 = UNCERTAINTY_MEASURE_WITH_UNIT (LENGTH_MEASURE( 1.000000000000000082E-05 ), #8594, 'distance_accuracy_value', 'NONE');
#1063 = DIRECTION ( 'NONE',  ( -1.000000000000000000, 0.000000000000000000, 0.000000000000000000 ) ) ;
#1064 = CARTESIAN_POINT ( 'NONE',  ( -2.500000000000000000, 3.061616997868383141E-16, -5.560532340533429263 ) ) ;
#1065 = DIRECTION ( 'NONE',  ( 0.000000000000000000, 1.000000000000000000, 0.000000000000000000 ) ) ;
#1066 = CARTESIAN_POINT ( 'NONE',  ( -73.62500000204839523, 44.30836144126050158, -25.81189881249999374 ) ) ;
#1067 = CARTESIAN_POINT ( 'NONE',  ( -73.25000000204838102, 80.81189881250001861, -10.69163855873949132 ) ) ;
#1068 = ORIENTED_EDGE ( 'NONE', *, *, #6473, .F. ) ;
#1069 = CARTESIAN_POINT ( 'NONE',  ( -77.46875000204839523, 80.81189881250000440, -1.580522963032174394E-15 ) ) ;
#1070 = ORIENTED_EDGE ( 'NONE', *, *, #9812, .T. ) ;
#1071 = CARTESIAN_POINT ( 'NONE',  ( -61.29696941632089846, 49.00264374128124700, 12.67759916065936743 ) ) ;
#1072 = EDGE_CURVE ( 'NONE', #2315, #4836, #4003, .T. ) ;
#1073 = AXIS2_PLACEMENT_3D ( 'NONE', #1210, #2957, #3857 ) ;
#1074 = CARTESIAN_POINT ( 'NONE',  ( -71.46802368722833876, 77.35376350879521112, 12.90594348738575903 ) ) ;
#1075 = CARTESIAN_POINT ( 'NONE',  ( -78.00000000000001421, 50.75735931288069480, -12.72791868944003824 ) ) ;
#1076 = EDGE_CURVE ( 'NONE', #3494, #10599, #10880, .T. ) ;
#1077 = FACE_OUTER_BOUND ( 'NONE', #11804, .T. ) ;
#1078 = ORIENTED_EDGE ( 'NONE', *, *, #7905, .F. ) ;
#1079 = PRODUCT_DEFINITION_SHAPE ( 'NONE', 'NONE',  #11859 ) ;
#1080 = VECTOR ( 'NONE', #11683, 1000.000000000000000 ) ;
#1081 = DIRECTION ( 'NONE',  ( -1.000000000000000000, 0.000000000000000000, 0.000000000000000000 ) ) ;
#1082 = CARTESIAN_POINT ( 'NONE',  ( -76.53125000409677625, 44.64466094067262958, 25.00000000000001066 ) ) ;
#1083 = AXIS2_PLACEMENT_3D ( 'NONE', #4052, #6635, #3924 ) ;
#1084 = DIRECTION ( 'NONE',  ( -0.000000000000000000, -0.000000000000000000, 1.000000000000000000 ) ) ;
#1085 = FACE_BOUND ( 'NONE', #2514, .T. ) ;
#1086 = CARTESIAN_POINT ( 'NONE',  ( -5.249611880419077892, 58.30742012212186154, -6.189572715011546933 ) ) ;
#1087 = CARTESIAN_POINT ( 'NONE',  ( -2.899087953157023723, 65.30046538299916392, -19.43989248047692442 ) ) ;
#1088 = CIRCLE ( 'NONE', #7236, 1.500000000000001332 ) ;
#1089 = CARTESIAN_POINT ( 'NONE',  ( 0.000000000000000000, -17.82799999999998875, -4.999999999999995559 ) ) ;
#1090 = ORIENTED_EDGE ( 'NONE', *, *, #6143, .T. ) ;
#1091 = CYLINDRICAL_SURFACE ( 'NONE', #6278, 1.500000000000000000 ) ;
#1092 = EDGE_CURVE ( 'NONE', #301, #7726, #4627, .T. ) ;
#1093 = LINE ( 'NONE', #10317, #4033 ) ;
#1094 = ORIENTED_EDGE ( 'NONE', *, *, #432, .T. ) ;
#1095 = CARTESIAN_POINT ( 'NONE',  ( 23.00000000000000000, 76.00000000000000000, 0.000000000000000000 ) ) ;
#1096 = CARTESIAN_POINT ( 'NONE',  ( -79.34375000204839523, 55.00000000000000000, -25.81189881249999729 ) ) ;
#1097 = AXIS2_PLACEMENT_3D ( 'NONE', #8579, #2100, #4867 ) ;
#1098 = CARTESIAN_POINT ( 'NONE',  ( 0.000000000000000000, 0.000000000000000000, -2.968018054819144158 ) ) ;
#1099 = CARTESIAN_POINT ( 'NONE',  ( -54.32961274566940801, 69.86573439484330095, 14.86481071665870601 ) ) ;
#1100 = CARTESIAN_POINT ( 'NONE',  ( -50.82691677660828589, 75.68920158268997511, 4.121780573430135597 ) ) ;
#1101 = ORIENTED_EDGE ( 'NONE', *, *, #298, .F. ) ;
#1102 = CARTESIAN_POINT ( 'NONE',  ( -78.00000000000002842, 38.02943725152282184, 3.371917797929946392E-06 ) ) ;
#1103 = DIRECTION ( 'NONE',  ( 0.000000000000000000, 0.000000000000000000, 1.000000000000000000 ) ) ;
#1104 = CARTESIAN_POINT ( 'NONE',  ( -80.00000000000000000, 55.00000000000000000, -24.99999999999999645 ) ) ;
#1105 = ORIENTED_EDGE ( 'NONE', *, *, #11853, .T. ) ;
#1106 = CARTESIAN_POINT ( 'NONE',  ( -18.26269090243636128, 68.34536746166378407, 16.25747718207173520 ) ) ;
#1107 = CARTESIAN_POINT ( 'NONE',  ( 7.127167418523728593, 42.78307170200208276, 7.042457608538825298 ) ) ;
#1108 = CARTESIAN_POINT ( 'NONE',  ( -20.00000000000003197, -57.00000000000000000, 5.000000000000000000 ) ) ;
#1109 = DIRECTION ( 'NONE',  ( -1.000000000000000000, -0.000000000000000000, -0.000000000000000000 ) ) ;
#1110 = EDGE_CURVE ( 'NONE', #5840, #8998, #2890, .T. ) ;
#1111 = CARTESIAN_POINT ( 'NONE',  ( 2.500000000000000000, 0.000000000000000000, -3.131981945180866589 ) ) ;
#1112 = DIRECTION ( 'NONE',  ( -0.000000000000000000, -0.000000000000000000, -1.000000000000000000 ) ) ;
#1113 = ADVANCED_BREP_SHAPE_REPRESENTATION ( '', ( #8587, #4738 ), #2442 ) ;
#1114 = VERTEX_POINT ( 'NONE', #1204 ) ;
#1115 = CARTESIAN_POINT ( 'NONE',  ( -79.62500000000000000, 80.00000000000000000, -1.530808498934191324E-15 ) ) ;
#1116 = CARTESIAN_POINT ( 'NONE',  ( -25.42602701123318099, 54.99834177037958938, 0.01637032750073019391 ) ) ;
#1117 = CARTESIAN_POINT ( 'NONE',  ( -36.46296276145401549, 52.49655656964354478, -4.331271186457903433 ) ) ;
#1118 = DIRECTION ( 'NONE',  ( -1.000000000000000000, -0.000000000000000000, -0.000000000000000000 ) ) ;
#1119 = CARTESIAN_POINT ( 'NONE',  ( -69.13100345326250817, 41.34467958230499107, 3.669940632046716278 ) ) ;
#1120 = AXIS2_PLACEMENT_3D ( 'NONE', #1648, #2557, #3689 ) ;
#1121 = ORIENTED_EDGE ( 'NONE', *, *, #9294, .F. ) ;
#1122 = CARTESIAN_POINT ( 'NONE',  ( -5.929357825456832209, 64.91315550346766372, -18.55154749960842153 ) ) ;
#1123 = FACE_OUTER_BOUND ( 'NONE', #11707, .T. ) ;
#1124 = CARTESIAN_POINT ( 'NONE',  ( -2.500000000000005773, -4.330127018922191873, -6.099999999999999645 ) ) ;
#1125 = FACE_OUTER_BOUND ( 'NONE', #2753, .T. ) ;
#1126 = CARTESIAN_POINT ( 'NONE',  ( -72.68750000204839523, 44.30836144126053000, 25.81189881250000795 ) ) ;
#1127 = CARTESIAN_POINT ( 'NONE',  ( -73.71875000204839523, 36.74823131438024859, -18.25176868561973720 ) ) ;
#1128 = ORIENTED_EDGE ( 'NONE', *, *, #8880, .T. ) ;
#1129 = CARTESIAN_POINT ( 'NONE',  ( -78.03125000409677625, 44.64466094067262958, 25.00000000000001066 ) ) ;
#1130 = AXIS2_PLACEMENT_3D ( 'NONE', #6175, #8085, #11658 ) ;
#1131 = ORIENTED_EDGE ( 'NONE', *, *, #4934, .T. ) ;
#1132 = CARTESIAN_POINT ( 'NONE',  ( 25.03499957223221628, 79.78147775635788719, -3.407189920745893108 ) ) ;
#1133 = CARTESIAN_POINT ( 'NONE',  ( -36.12710455038816093, 46.37784419364835742, -11.21156427467630223 ) ) ;
#1134 = CARTESIAN_POINT ( 'NONE',  ( -79.53125000204838102, 55.00000000000000000, -25.81189881249999729 ) ) ;
#1135 = CARTESIAN_POINT ( 'NONE',  ( -75.00000000000001421, 80.11351121041060708, 2.705448568323045144 ) ) ;
#1136 = DIRECTION ( 'NONE',  ( 1.000000000000000000, 0.000000000000000000, 0.000000000000000000 ) ) ;
#1137 = AXIS2_PLACEMENT_3D ( 'NONE', #1291, #3153, #8722 ) ;
#1138 = ORIENTED_EDGE ( 'NONE', *, *, #8425, .F. ) ;
#1139 = CARTESIAN_POINT ( 'NONE',  ( -78.40625000000000000, 65.35533905932737753, -24.99999999999999645 ) ) ;
#1140 = CARTESIAN_POINT ( 'NONE',  ( -73.53125000409676204, 44.64466094067262958, 25.00000000000001066 ) ) ;
#1141 = DIRECTION ( 'NONE',  ( 0.000000000000000000, 0.4999997706924120822, -0.8660255361751958425 ) ) ;
#1142 = FACE_BOUND ( 'NONE', #2463, .T. ) ;
#1143 = EDGE_CURVE ( 'NONE', #3987, #494, #8398, .T. ) ;
#1144 = CARTESIAN_POINT ( 'NONE',  ( 0.7765813511237322775, 51.48435031992290334, -6.093068385610369120 ) ) ;
#1145 = LINE ( 'NONE', #7519, #1367 ) ;
#1146 = ADVANCED_FACE ( 'NONE', ( #182 ), #11647, .F. ) ;
#1147 = CARTESIAN_POINT ( 'NONE',  ( -2.500000000000000000, 3.061616997868383141E-16, -3.832189483390572970 ) ) ;
#1148 = ORIENTED_EDGE ( 'NONE', *, *, #2304, .F. ) ;
#1149 = CYLINDRICAL_SURFACE ( 'NONE', #8557, 1.499999999999999556 ) ;
#1150 = AXIS2_PLACEMENT_3D ( 'NONE', #7485, #1112, #2137 ) ;
#1151 = DIRECTION ( 'NONE',  ( 1.000000000000000000, 0.000000000000000000, 0.000000000000000000 ) ) ;
#1152 = EDGE_CURVE ( 'NONE', #8509, #1264, #2669, .T. ) ;
#1153 = VERTEX_POINT ( 'NONE', #101 ) ;
#1154 = CARTESIAN_POINT ( 'NONE',  ( -42.33720994522852266, 55.00043528610386545, -21.02753041772728437 ) ) ;
#1155 = AXIS2_PLACEMENT_3D ( 'NONE', #5306, #2664, #4410 ) ;
#1156 = CARTESIAN_POINT ( 'NONE',  ( -74.37500000204838102, 80.81189881250001861, 10.69163855873948599 ) ) ;
#1157 = CARTESIAN_POINT ( 'NONE',  ( 5.000000000000000888, 0.9828435001097619583, -0.04309034703445715347 ) ) ;
#1158 = CARTESIAN_POINT ( 'NONE',  ( -80.00000000000002842, 59.24264068711927678, 12.72792543327563131 ) ) ;
#1159 = VECTOR ( 'NONE', #10817, 1000.000000000000000 ) ;
#1160 = CIRCLE ( 'NONE', #4437, 2.500000000000000000 ) ;
#1161 = DIRECTION ( 'NONE',  ( -0.8191520442889974607, 0.000000000000000000, -0.5735764363510379438 ) ) ;
#1162 = ORIENTED_EDGE ( 'NONE', *, *, #1324, .F. ) ;
#1163 = FACE_OUTER_BOUND ( 'NONE', #7901, .T. ) ;
#1164 = CARTESIAN_POINT ( 'NONE',  ( -8.481641943402102868, 57.21203007224725212, -4.487076300782732119 ) ) ;
#1165 = PRODUCT_RELATED_PRODUCT_CATEGORY ( 'part', '', ( #1453 ) ) ;
#1166 = CARTESIAN_POINT ( 'NONE',  ( 3.451907635234679361, 34.19915017745972108, -3.085386652995293133 ) ) ;
#1167 = ORIENTED_EDGE ( 'NONE', *, *, #4525, .F. ) ;
#1168 = EDGE_CURVE ( 'NONE', #8716, #7813, #8354, .T. ) ;
#1169 = CARTESIAN_POINT ( 'NONE',  ( -53.54812715265580181, 73.03736663818040142, 10.81090271242882039 ) ) ;
#1170 = AXIS2_PLACEMENT_3D ( 'NONE', #593, #1385, #5046 ) ;
#1171 = CARTESIAN_POINT ( 'NONE',  ( 21.12703399079512323, 68.61832863460267617, 3.659187381993185717 ) ) ;
#1172 = AXIS2_PLACEMENT_3D ( 'NONE', #5050, #537, #4201 ) ;
#1173 = CARTESIAN_POINT ( 'NONE',  ( -5.000000000000000000, -0.9724665692850883447, -0.04193043885209645633 ) ) ;
#1174 = CYLINDRICAL_SURFACE ( 'NONE', #4688, 1.499999999999999556 ) ;
#1175 = CARTESIAN_POINT ( 'NONE',  ( -15.00000000000000355, 0.000000000000000000, 30.00000000000000711 ) ) ;
#1176 = LINE ( 'NONE', #217, #961 ) ;
#1177 = ORIENTED_EDGE ( 'NONE', *, *, #5340, .T. ) ;
#1178 = CARTESIAN_POINT ( 'NONE',  ( -78.21875000000001421, 80.00000000000001421, -10.35533905932737753 ) ) ;
#1179 = CARTESIAN_POINT ( 'NONE',  ( -63.46281172795519154, 55.00260107563563139, -0.003976208690220505923 ) ) ;
#1180 = DIRECTION ( 'NONE',  ( -1.000000000000000000, -0.000000000000000000, -0.000000000000000000 ) ) ;
#1181 = EDGE_CURVE ( 'NONE', #10867, #4978, #10110, .T. ) ;
#1182 = EDGE_CURVE ( 'NONE', #3322, #7121, #8405, .T. ) ;
#1183 = AXIS2_PLACEMENT_3D ( 'NONE', #6561, #7279, #2718 ) ;
#1184 =( NAMED_UNIT ( * ) SI_UNIT ( $, .STERADIAN. ) SOLID_ANGLE_UNIT ( ) );
#1185 = CARTESIAN_POINT ( 'NONE',  ( 0.000000000000000000, 0.000000000000000000, -1.753742857142857048 ) ) ;
#1186 = CARTESIAN_POINT ( 'NONE',  ( -55.78867880362859921, 66.25575517429669503, 8.346979382912829593 ) ) ;
#1187 = EDGE_LOOP ( 'NONE', ( #9606, #9183 ) ) ;
#1188 = CARTESIAN_POINT ( 'NONE',  ( -4.160267277967630406, 59.12176995062825569, -20.68921489609442332 ) ) ;
#1189 = DIRECTION ( 'NONE',  ( -1.000000000000000000, 0.000000000000000000, 0.000000000000000000 ) ) ;
#1190 = CARTESIAN_POINT ( 'NONE',  ( 53.00000000000000000, 105.0000000000000142, -6.000000000000000000 ) ) ;
#1191 = EDGE_CURVE ( 'NONE', #1730, #6384, #8567, .T. ) ;
#1192 = DIRECTION ( 'NONE',  ( -1.000000000000000000, -0.000000000000000000, -0.000000000000000000 ) ) ;
#1193 = CARTESIAN_POINT ( 'NONE',  ( -22.63432272110139110, 77.75090647838392499, 10.39239001733118783 ) ) ;
#1194 = CARTESIAN_POINT ( 'NONE',  ( -79.15625000204839523, 73.25176868561975141, -18.25176868561974430 ) ) ;
#1195 = VERTEX_POINT ( 'NONE', #7671 ) ;
#1196 = CARTESIAN_POINT ( 'NONE',  ( -71.40810441781462714, 80.81189881250000440, 6.916273779317701376 ) ) ;
#1197 = DIRECTION ( 'NONE',  ( -1.000000000000000000, -6.033820786006286457E-17, -0.000000000000000000 ) ) ;
#1198 = CARTESIAN_POINT ( 'NONE',  ( 24.58810204984513348, 79.39961546340161647, -5.461861930764240647 ) ) ;
#1199 = CARTESIAN_POINT ( 'NONE',  ( -67.21123314643752167, 41.02399581862376721, 1.828645404196747037 ) ) ;
#1200 = CARTESIAN_POINT ( 'NONE',  ( 0.000000000000000000, 0.000000000000000000, -2.267810516609437776 ) ) ;
#1201 = CARTESIAN_POINT ( 'NONE',  ( -75.00000000000000000, 78.13883143010173171, -10.47133000126702917 ) ) ;
#1202 = CARTESIAN_POINT ( 'NONE',  ( -78.00000000000002842, 50.75735931288069480, 4.242644059037076865 ) ) ;
#1203 = ORIENTED_EDGE ( 'NONE', *, *, #2554, .F. ) ;
#1204 = CARTESIAN_POINT ( 'NONE',  ( 52.99999999999999289, 58.53553390593273065, -3.535533905932738197 ) ) ;
#1205 = CARTESIAN_POINT ( 'NONE',  ( -74.18750000409677625, 72.67766952966368876, -17.67766952966368876 ) ) ;
#1206 = LINE ( 'NONE', #5960, #6 ) ;
#1207 = ORIENTED_EDGE ( 'NONE', *, *, #3224, .T. ) ;
#1208 = CARTESIAN_POINT ( 'NONE',  ( -16.04203362689861834, 60.18690525748159814, 4.700552706782350931 ) ) ;
#1209 = CARTESIAN_POINT ( 'NONE',  ( -72.50000000000000000, 55.00000000000000000, -24.99999999999999645 ) ) ;
#1210 = CARTESIAN_POINT ( 'NONE',  ( 52.99999999999999289, 55.00000000000000000, 0.000000000000000000 ) ) ;
#1211 = ORIENTED_EDGE ( 'NONE', *, *, #75, .T. ) ;
#1212 = FACE_OUTER_BOUND ( 'NONE', #9717, .T. ) ;
#1213 = CARTESIAN_POINT ( 'NONE',  ( -78.78125000204838102, 55.00000000000000000, 25.81189881249999729 ) ) ;
#1214 = EDGE_LOOP ( 'NONE', ( #11185, #4171, #3721, #9359 ) ) ;
#1215 = CARTESIAN_POINT ( 'NONE',  ( -53.69727390230763575, 74.79022971164903311, 7.081167078663678893 ) ) ;
#1216 = CARTESIAN_POINT ( 'NONE',  ( -71.56250000204838102, 80.81189881250001861, -10.69163855873949132 ) ) ;
#1217 = CARTESIAN_POINT ( 'NONE',  ( 4.999999999999999112, 0.4881033300985036516, 4.535861432546776344E-16 ) ) ;
#1218 = CARTESIAN_POINT ( 'NONE',  ( -54.63607242817042930, 69.12530316040908929, 15.58420556269393309 ) ) ;
#1219 = CARTESIAN_POINT ( 'NONE',  ( -77.93750000409679046, 37.32233047033631124, 17.67766952966369232 ) ) ;
#1220 = EDGE_LOOP ( 'NONE', ( #9174, #10799, #9543, #8141, #4587, #5459, #10657, #5694, #7579, #2967, #800, #10288, #2333, #138 ) ) ;
#1221 = FACE_OUTER_BOUND ( 'NONE', #11308, .T. ) ;
#1222 = CARTESIAN_POINT ( 'NONE',  ( -6.544209565228709558, 55.65803961495722518, -4.967200339763780725 ) ) ;
#1223 = CARTESIAN_POINT ( 'NONE',  ( -78.12500000000004263, 79.99999999999992895, -1.530808498934187183E-15 ) ) ;
#1224 = ORIENTED_EDGE ( 'NONE', *, *, #197, .F. ) ;
#1225 = ADVANCED_FACE ( 'NONE', ( #11306, #3116 ), #6782, .T. ) ;
#1226 = CARTESIAN_POINT ( 'NONE',  ( -61.40197252463548239, 48.89621197884387982, 20.10936848441244607 ) ) ;
#1227 = CARTESIAN_POINT ( 'NONE',  ( 9.460426116349054837, 46.40793895553105131, 11.18147790519370766 ) ) ;
#1228 = CARTESIAN_POINT ( 'NONE',  ( -78.50000000000000000, 55.00000000000000000, -24.99999999999999645 ) ) ;
#1229 = CARTESIAN_POINT ( 'NONE',  ( -78.00000000000001421, 59.24264068711927678, -2.742637315201482462 ) ) ;
#1230 = CARTESIAN_POINT ( 'NONE',  ( -18.99070286106124428, 58.97347284273117651, 3.052796309671656161 ) ) ;
#1231 = CARTESIAN_POINT ( 'NONE',  ( -75.00000000000001421, 76.68791387293471473, 12.43520775219157315 ) ) ;
#1232 = ORIENTED_EDGE ( 'NONE', *, *, #946, .F. ) ;
#1233 = CARTESIAN_POINT ( 'NONE',  ( -79.06250000000001421, 37.32233047033631124, 17.67766952966369232 ) ) ;
#1234 = CARTESIAN_POINT ( 'NONE',  ( -74.99999999999997158, 42.18634379380805655, -22.42280631998790597 ) ) ;
#1235 =( GEOMETRIC_REPRESENTATION_CONTEXT ( 3 ) GLOBAL_UNCERTAINTY_ASSIGNED_CONTEXT ( ( #3433 ) ) GLOBAL_UNIT_ASSIGNED_CONTEXT ( ( #11335, #6810, #5979 ) ) REPRESENTATION_CONTEXT ( 'NONE', 'WORKASPACE' ) );
#1236 = CARTESIAN_POINT ( 'NONE',  ( -80.00000000000001421, 59.24264068711927678, -4.242637315201482906 ) ) ;
#1237 = FACE_OUTER_BOUND ( 'NONE', #7141, .T. ) ;
#1238 = CARTESIAN_POINT ( 'NONE',  ( 1.042054107055792711, 48.65947148651063259, -2.999074899036769271 ) ) ;
#1239 = ORIENTED_EDGE ( 'NONE', *, *, #9815, .F. ) ;
#1240 = CARTESIAN_POINT ( 'NONE',  ( -15.82693394478133797, 72.53700911420227726, 11.72543866452437733 ) ) ;
#1241 = CARTESIAN_POINT ( 'NONE',  ( -2.500000000000003553, 4.330127018922192761, -6.099999999999999645 ) ) ;
#1242 = EDGE_CURVE ( 'NONE', #9881, #10478, #2712, .T. ) ;
#1243 = DIRECTION ( 'NONE',  ( 0.000000000000000000, 0.000000000000000000, 1.000000000000000000 ) ) ;
#1244 = DIRECTION ( 'NONE',  ( -1.000000000000000000, -0.000000000000000000, -0.000000000000000000 ) ) ;
#1245 = CARTESIAN_POINT ( 'NONE',  ( -2.976011536945806224, 65.72704692019560468, 22.58178635561741032 ) ) ;
#1246 = CARTESIAN_POINT ( 'NONE',  ( -77.18750000204839523, 65.69163855873949842, 25.81189881250000440 ) ) ;
#1247 = AXIS2_PLACEMENT_3D ( 'NONE', #5557, #1050, #3815 ) ;
#1248 = ORIENTED_EDGE ( 'NONE', *, *, #10185, .F. ) ;
#1249 = CARTESIAN_POINT ( 'NONE',  ( -77.93750000409679046, 37.32233047033631124, 17.67766952966369232 ) ) ;
#1250 = ORIENTED_EDGE ( 'NONE', *, *, #4162, .T. ) ;
#1251 = DIRECTION ( 'NONE',  ( 0.000000000000000000, 1.000000000000000000, 0.000000000000000000 ) ) ;
#1252 = CARTESIAN_POINT ( 'NONE',  ( -36.87283257201146114, 47.96004688000734006, -12.21088183946608119 ) ) ;
#1253 = EDGE_CURVE ( 'NONE', #10987, #5798, #9862, .T. ) ;
#1254 = DIRECTION ( 'NONE',  ( -1.000000000000000000, 0.000000000000000000, 0.000000000000000000 ) ) ;
#1255 = FACE_OUTER_BOUND ( 'NONE', #2174, .T. ) ;
#1256 = CARTESIAN_POINT ( 'NONE',  ( 0.000000000000000000, 0.000000000000000000, -6.099999999999999645 ) ) ;
#1257 = ORIENTED_EDGE ( 'NONE', *, *, #6099, .T. ) ;
#1258 = AXIS2_PLACEMENT_3D ( 'NONE', #7063, #7123, #10746 ) ;
#1259 = CARTESIAN_POINT ( 'NONE',  ( -76.15624999999998579, 44.64466094067262958, 25.00000000000001066 ) ) ;
#1260 = CARTESIAN_POINT ( 'NONE',  ( -74.65625000409679046, 30.00000000000000355, -10.35533905932738108 ) ) ;
#1261 =( BOUNDED_CURVE ( )  B_SPLINE_CURVE ( 2, ( #11742, #1796, #8158, #4329, #4505, #8218, #3605, #10900, #9834 ),
 .UNSPECIFIED., .F., .T. ) 
 B_SPLINE_CURVE_WITH_KNOTS ( ( 3, 2, 2, 2, 3 ),
 ( 0.1666666666666667962, 0.1875000000000001665, 0.2083333333333335369, 0.2291666666666668517, 0.2500000000000002220 ),
 .UNSPECIFIED. ) 
 CURVE ( )  GEOMETRIC_REPRESENTATION_ITEM ( )  RATIONAL_B_SPLINE_CURVE ( ( 0.9999999999999994449, 0.9238795325112872936, 1.000000000000000000, 0.9238795325112867385, 1.000000000000000000, 0.9238795325112867385, 1.000000000000000000, 0.9238795325112859613, 1.000000000000000888 ) ) 
 REPRESENTATION_ITEM ( '' )  );
#1262 = VECTOR ( 'NONE', #11203, 1000.000000000000000 ) ;
#1263 = CARTESIAN_POINT ( 'NONE',  ( -48.15199486393218109, 58.76922744225378636, -3.301526873569539777 ) ) ;
#1264 = VERTEX_POINT ( 'NONE', #11719 ) ;
#1265 = B_SPLINE_CURVE_WITH_KNOTS ( 'NONE', 3,
 ( #4283, #4224, #11516, #1524, #7886, #1350, #5072, #444 ),
 .UNSPECIFIED., .F., .F.,
 ( 4, 2, 2, 4 ),
 ( 0.002921158011986725936, 0.003648658599403077456, 0.004376159186819428108, 0.005831160361652132015 ),
 .UNSPECIFIED. ) ;
#1266 = CARTESIAN_POINT ( 'NONE',  ( -4.666526940154917646, 57.68340530217055573, -6.477642677762205814 ) ) ;
#1267 = CARTESIAN_POINT ( 'NONE',  ( 14.99999999999999645, 5.000000000000000000, 30.00000000000000711 ) ) ;
#1268 = CIRCLE ( 'NONE', #3564, 2.500000000000000000 ) ;
#1269 = LINE ( 'NONE', #10251, #1262 ) ;
#1270 = EDGE_LOOP ( 'NONE', ( #9513, #11457 ) ) ;
#1271 = LINE ( 'NONE', #4940, #1848 ) ;
#1272 = CARTESIAN_POINT ( 'NONE',  ( -76.43750000204838102, 65.69163855873948421, -25.81189881250000084 ) ) ;
#1273 = ORIENTED_EDGE ( 'NONE', *, *, #5965, .F. ) ;
#1274 = EDGE_CURVE ( 'NONE', #2004, #9652, #8220, .T. ) ;
#1275 = CARTESIAN_POINT ( 'NONE',  ( -60.69833702282029009, 56.03208645306531110, 20.99415308669729541 ) ) ;
#1276 = CARTESIAN_POINT ( 'NONE',  ( -73.34375000204839523, 55.00000000000000000, -25.81189881249999729 ) ) ;
#1277 = DIRECTION ( 'NONE',  ( -1.000000000000000000, -0.000000000000000000, -0.000000000000000000 ) ) ;
#1278 = DIRECTION ( 'NONE',  ( 0.000000000000000000, 1.000000000000000000, 0.000000000000000000 ) ) ;
#1279 = AXIS2_PLACEMENT_3D ( 'NONE', #7664, #3219, #3045 ) ;
#1280 = FILL_AREA_STYLE ('',( #9367 ) ) ;
#1281 = AXIS2_PLACEMENT_3D ( 'NONE', #8097, #9101, #4381 ) ;
#1282 = LINE ( 'NONE', #10265, #7592 ) ;
#1283 = ORIENTED_EDGE ( 'NONE', *, *, #7410, .T. ) ;
#1284 = CARTESIAN_POINT ( 'NONE',  ( -72.31250000204839523, 29.18810118750000981, 10.69163855873950020 ) ) ;
#1285 = DIRECTION ( 'NONE',  ( -1.000000000000000000, -0.000000000000000000, -0.000000000000000000 ) ) ;
#1286 = CARTESIAN_POINT ( 'NONE',  ( -45.83980951013849392, 66.71822699054862937, -17.55167914569291554 ) ) ;
#1287 = ORIENTED_EDGE ( 'NONE', *, *, #3917, .F. ) ;
#1288 = CARTESIAN_POINT ( 'NONE',  ( -1.189062444204875835, 44.43480771519530492, -18.33185415547853481 ) ) ;
#1289 = VECTOR ( 'NONE', #8219, 1000.000000000000000 ) ;
#1290 = CARTESIAN_POINT ( 'NONE',  ( -43.21475900837984341, 58.08538667521604282, -20.80084980650556759 ) ) ;
#1291 = CARTESIAN_POINT ( 'NONE',  ( -78.00000000000001421, 63.48528137423857487, 3.371917795327861178E-06 ) ) ;
#1292 = DIRECTION ( 'NONE',  ( 1.000000000000000000, 6.033820786006286457E-17, 0.000000000000000000 ) ) ;
#1293 = VECTOR ( 'NONE', #9725, 1000.000000000000000 ) ;
#1294 = EDGE_CURVE ( 'NONE', #322, #6131, #3340, .T. ) ;
#1295 = DIRECTION ( 'NONE',  ( -1.000000000000000000, -0.000000000000000000, -0.000000000000000000 ) ) ;
#1296 = ORIENTED_EDGE ( 'NONE', *, *, #9433, .T. ) ;
#1297 = CARTESIAN_POINT ( 'NONE',  ( -76.62500000000000000, 80.00000000000000000, -1.530808498934191324E-15 ) ) ;
#1298 = DIRECTION ( 'NONE',  ( -0.04813578311308589625, -0.9988407004187033200, 0.0004489667737563936712 ) ) ;
#1299 = LINE ( 'NONE', #4722, #6694 ) ;
#1300 = AXIS2_PLACEMENT_3D ( 'NONE', #7858, #10536, #10591 ) ;
#1301 = CARTESIAN_POINT ( 'NONE',  ( -80.00000000000001421, 42.27207793864211283, -12.72791868944003824 ) ) ;
#1302 = CARTESIAN_POINT ( 'NONE',  ( -31.91627726477343074, 48.28752732786880841, 2.036885257361992441 ) ) ;
#1303 = ORIENTED_EDGE ( 'NONE', *, *, #1182, .F. ) ;
#1304 = CARTESIAN_POINT ( 'NONE',  ( -53.73751484135783585, 71.24472392590685388, 13.33357819947211453 ) ) ;
#1305 = CARTESIAN_POINT ( 'NONE',  ( 19.99999999999996803, -63.00000000000000000, 5.000000000000000000 ) ) ;
#1306 = ADVANCED_FACE ( 'NONE', ( #9805 ), #10699, .F. ) ;
#1307 = DIRECTION ( 'NONE',  ( 0.000000000000000000, 1.000000000000000000, 0.000000000000000000 ) ) ;
#1308 = EDGE_CURVE ( 'NONE', #1419, #6608, #6316, .T. ) ;
#1309 = CARTESIAN_POINT ( 'NONE',  ( -75.40625000204839523, 36.74823131438026280, 18.25176868561974786 ) ) ;
#1310 = CARTESIAN_POINT ( 'NONE',  ( -24.23439331329375790, 79.09827848464085776, -6.702477181294344000 ) ) ;
#1311 = CARTESIAN_POINT ( 'NONE',  ( -72.78125000204838102, 55.00000000000000000, 25.81189881249999729 ) ) ;
#1312 = VERTEX_POINT ( 'NONE', #640 ) ;
#1313 = CARTESIAN_POINT ( 'NONE',  ( -77.84375000409677625, 30.00000000000001421, 10.35533905932739174 ) ) ;
#1314 = ORIENTED_EDGE ( 'NONE', *, *, #7805, .F. ) ;
#1315 = CARTESIAN_POINT ( 'NONE',  ( -1.477628194636992243, 49.49121550494065502, -20.47411891050684218 ) ) ;
#1316 = EDGE_CURVE ( 'NONE', #1730, #5840, #4967, .T. ) ;
#1317 = DIRECTION ( 'NONE',  ( -1.000000000000000000, 0.000000000000000000, -0.000000000000000000 ) ) ;
#1318 = AXIS2_PLACEMENT_3D ( 'NONE', #8730, #6167, #10625 ) ;
#1319 = CARTESIAN_POINT ( 'NONE',  ( -74.99999999999997158, 77.69762738690542392, 10.61382896765898209 ) ) ;
#1320 = DIRECTION ( 'NONE',  ( 0.000000000000000000, 1.000000000000000000, 0.000000000000000000 ) ) ;
#1321 = EDGE_CURVE ( 'NONE', #10439, #8197, #10496, .T. ) ;
#1322 = VERTEX_POINT ( 'NONE', #11595 ) ;
#1323 = ADVANCED_FACE ( 'NONE', ( #6058 ), #4481, .T. ) ;
#1324 = EDGE_CURVE ( 'NONE', #430, #96, #1885, .T. ) ;
#1325 = AXIS2_PLACEMENT_3D ( 'NONE', #1490, #2447, #7907 ) ;
#1326 = CARTESIAN_POINT ( 'NONE',  ( -72.50000000000000000, 55.00000000000000000, -24.99999999999999645 ) ) ;
#1327 = CARTESIAN_POINT ( 'NONE',  ( -74.00000000409677625, 80.00000000000000000, -1.530808498934191324E-15 ) ) ;
#1328 = AXIS2_PLACEMENT_3D ( 'NONE', #3473, #2386, #8089 ) ;
#1329 = LINE ( 'NONE', #4992, #5381 ) ;
#1330 = ORIENTED_EDGE ( 'NONE', *, *, #4547, .T. ) ;
#1331 = CARTESIAN_POINT ( 'NONE',  ( 4.666531114835057892, 48.52758949912974629, -2.680605614690282579 ) ) ;
#1332 = EDGE_CURVE ( 'NONE', #8286, #8080, #3287, .T. ) ;
#1333 = ADVANCED_FACE ( 'NONE', ( #8020 ), #5928, .F. ) ;
#1334 = CARTESIAN_POINT ( 'NONE',  ( -78.00000000000001421, 63.48528137423857487, -9.985278002320759683 ) ) ;
#1335 = AXIS2_PLACEMENT_3D ( 'NONE', #3104, #11347, #6769 ) ;
#1336 = CARTESIAN_POINT ( 'NONE',  ( -75.87500000409677625, 55.00000000000000000, -24.99999999999999645 ) ) ;
#1337 = ADVANCED_FACE ( 'NONE', ( #696 ), #9747, .T. ) ;
#1338 = ORIENTED_EDGE ( 'NONE', *, *, #2939, .F. ) ;
#1339 = CARTESIAN_POINT ( 'NONE',  ( 10.64825151755819022, 68.66818062749433693, 17.26560489676726462 ) ) ;
#1340 = B_SPLINE_CURVE_WITH_KNOTS ( 'NONE', 3,
 ( #4066, #4114, #7773, #1234, #11351, #11403, #3216, #8729, #4903, #6884, #2982, #10281, #5750, #9385, #8555 ),
 .UNSPECIFIED., .F., .F.,
 ( 4, 2, 1, 2, 2, 2, 2, 4 ),
 ( 2.418898813002652444E-15, 0.002548748984084002640, 0.005097497968165586209, 0.007646246952247169777, 0.01019499593632875248, 0.01529249390449191962, 0.01784124288857351706, 0.02038999187265511104 ),
 .UNSPECIFIED. ) ;
#1341 = CARTESIAN_POINT ( 'NONE',  ( -75.68750000204838102, 44.30836144126052289, 25.81189881250000795 ) ) ;
#1342 = VERTEX_POINT ( 'NONE', #7074 ) ;
#1343 = CARTESIAN_POINT ( 'NONE',  ( -52.82691659388441252, 75.69008924411679118, 4.122156975067814422 ) ) ;
#1344 = CARTESIAN_POINT ( 'NONE',  ( -75.21875000204839523, 29.18810118750000271, 4.741568889096522788E-15 ) ) ;
#1345 = LINE ( 'NONE', #5009, #6940 ) ;
#1346 = CARTESIAN_POINT ( 'NONE',  ( 0.000000000000000000, -17.82799999999998875, -4.999999999999995559 ) ) ;
#1347 = SURFACE_STYLE_USAGE ( .BOTH. , #2122 ) ;
#1348 = CARTESIAN_POINT ( 'NONE',  ( 0.000000000000000000, 0.000000000000000000, -6.099999999999999645 ) ) ;
#1349 = ORIENTED_EDGE ( 'NONE', *, *, #4258, .F. ) ;
#1350 = CARTESIAN_POINT ( 'NONE',  ( -4.180704885107416224, -3.359771601077114589, -0.1983443223721613746 ) ) ;
#1351 = CIRCLE ( 'NONE', #1733, 5.000000000000000888 ) ;
#1352 = CARTESIAN_POINT ( 'NONE',  ( -18.69730990872651333, 70.57397863033268948, 14.11552877426516339 ) ) ;
#1353 = ORIENTED_EDGE ( 'NONE', *, *, #1402, .T. ) ;
#1354 = CARTESIAN_POINT ( 'NONE',  ( 1.493523987181155643, 37.44802286055433171, -11.71834779115162561 ) ) ;
#1355 = CARTESIAN_POINT ( 'NONE',  ( -5.928718717905509195, 56.37336801400213915, -14.01350978889703391 ) ) ;
#1356 = LINE ( 'NONE', #5861, #6889 ) ;
#1357 = FACE_OUTER_BOUND ( 'NONE', #3937, .T. ) ;
#1358 = AXIS2_PLACEMENT_3D ( 'NONE', #10716, #3305, #9829 ) ;
#1359 = CARTESIAN_POINT ( 'NONE',  ( -78.00000000000002842, 46.51471862576140381, 1.500003371917798756 ) ) ;
#1360 = ORIENTED_EDGE ( 'NONE', *, *, #1799, .T. ) ;
#1361 = CARTESIAN_POINT ( 'NONE',  ( -74.00000000000000000, 55.00000000000000000, -24.99999999999999645 ) ) ;
#1362 = CARTESIAN_POINT ( 'NONE',  ( -64.33684479406403511, 55.00260128198466703, -0.002143347410900310612 ) ) ;
#1363 = VECTOR ( 'NONE', #5696, 1000.000000000000000 ) ;
#1364 = B_SPLINE_CURVE_WITH_KNOTS ( 'NONE', 3,
 ( #3453, #5314, #3388, #9683, #6163, #8073, #11709, #5372, #569, #743, #4237, #8904, #7895, #11525, #6104, #9796, #9735, #1533, #4292, #1589, #7950, #4359, #11644, #10138, #17, #10863, #915, #802, #7293, #9249, #5669, #8184, #7473, #6448, #10974, #4473, #136, #3627, #6575, #1763, #3800, #4644, #10079, #1815, #5429, #8125, #5610, #1997, #10204, #1037, #1876, #5485, #10925, #11762, #11094, #2908, #8296, #3569, #6338, #1941, #982, #2736, #7240, #2673, #77, #9970, #9078, #856, #6393, #4528, #11820, #10022, #3738, #9134, #4585, #8240, #8352, #4704, #3686, #7351, #5547, #7405, #2786, #9190, #11032, #2842, #6511, #199, #2300, #4762, #11334, #10325, #9308, #6809, #3868, #8480, #256, #2062, #6755, #8417, #9428, #6632, #7643, #1099, #1218, #10261, #319, #7528, #7704, #5731, #3984, #380, #11275, #4046, #3143, #9366, #3086, #4948, #10384, #6871, #2965, #10436, #2238, #11150 ),
 .UNSPECIFIED., .F., .F.,
 ( 4, 2, 2, 2, 2, 2, 2, 2, 2, 2, 2, 2, 2, 2, 2, 2, 2, 2, 2, 2, 2, 2, 2, 2, 2, 2, 2, 2, 2, 2, 2, 2, 2, 2, 2, 2, 2, 2, 2, 2, 2, 2, 2, 2, 2, 2, 2, 2, 2, 2, 2, 2, 2, 2, 2, 2, 2, 2, 2, 2, 2, 4 ),
 ( 0.000000000000000000, 0.02499977550252127645, 0.04999988577693819519, 0.07499999605135511394, 0.09999999831535408279, 0.1250000005793530378, 0.1500000028441162425, 0.1750000051088794195, 0.1937500039558066045, 0.2031250033792701970, 0.2125000028027338173, 0.2218750022261974375, 0.2312500016496610300, 0.2500000004965882150, 0.2750000027613288545, 0.3000000050260694384, 0.3187500038730080032, 0.3281250032964772578, 0.3375000027199465125, 0.3468750021434158226, 0.3562500015668850772, 0.3750000004138236420, 0.4000000026785641705, 0.4250000049433046989, 0.4437500037902432082, 0.4531250032137125183, 0.4625000026371817730, 0.4718750020606510276, 0.4812500014841203377, 0.5000000003310588470, 0.5250000025957997085, 0.5500000048605405700, 0.5687500037074788573, 0.5781250031309480564, 0.5875000025544172555, 0.5968750019778864546, 0.6062500014013556537, 0.6250000002482940520, 0.6500000025128280789, 0.6750000047773621059, 0.6937500036244039769, 0.7031250030479249125, 0.7125000024714458480, 0.7218750018949667835, 0.7312500013184877190, 0.7500000001655295900, 0.7750000023794885173, 0.8000000045934475557, 0.8187500034657768655, 0.8281250029019414649, 0.8375000023381060643, 0.8468750017742707747, 0.8562500012104353742, 0.8750000000827646840, 0.8937502654913498379, 0.9031253981956424148, 0.9125005308999349918, 0.9218756636042275687, 0.9312507963085201457, 0.9500010617171052996, 0.9750005308585526498, 1.000000000000000000 ),
 .UNSPECIFIED. ) ;
#1365 = FACE_OUTER_BOUND ( 'NONE', #11648, .T. ) ;
#1366 = AXIS2_PLACEMENT_3D ( 'NONE', #3867, #255, #11093 ) ;
#1367 = VECTOR ( 'NONE', #10249, 1000.000000000000000 ) ;
#1368 = DIRECTION ( 'NONE',  ( 0.000000000000000000, 0.000000000000000000, 1.000000000000000000 ) ) ;
#1369 = CARTESIAN_POINT ( 'NONE',  ( -43.58294393097721553, 55.68691547946620801, -6.980998355533345467 ) ) ;
#1370 = ORIENTED_EDGE ( 'NONE', *, *, #2171, .F. ) ;
#1371 = CARTESIAN_POINT ( 'NONE',  ( -29.54809237377008202, 34.60091625530366599, 5.109976345715927515 ) ) ;
#1372 = CARTESIAN_POINT ( 'NONE',  ( 0.000000000000000000, 0.000000000000000000, -1.753742857142857048 ) ) ;
#1373 = LINE ( 'NONE', #11304, #11545 ) ;
#1374 = CARTESIAN_POINT ( 'NONE',  ( -78.50000000204842365, 44.30836144126052289, 25.81189881250000795 ) ) ;
#1375 = CARTESIAN_POINT ( 'NONE',  ( -8.896007692468192118, 67.93420365865686961, 21.39919931194891944 ) ) ;
#1376 = CARTESIAN_POINT ( 'NONE',  ( -72.50000000204839523, 44.30836144126053000, 25.81189881250000795 ) ) ;
#1377 = ORIENTED_EDGE ( 'NONE', *, *, #7805, .T. ) ;
#1378 = AXIS2_PLACEMENT_3D ( 'NONE', #4847, #221, #3884 ) ;
#1379 = CARTESIAN_POINT ( 'NONE',  ( -76.53125000409677625, 44.64466094067262958, 25.00000000000001066 ) ) ;
#1380 = FACE_BOUND ( 'NONE', #6482, .T. ) ;
#1381 = AXIS2_PLACEMENT_3D ( 'NONE', #11447, #7816, #6146 ) ;
#1382 = FACE_BOUND ( 'NONE', #8062, .T. ) ;
#1383 = DIRECTION ( 'NONE',  ( 1.000000000000000000, 0.000000000000000000, 0.000000000000000000 ) ) ;
#1384 = CARTESIAN_POINT ( 'NONE',  ( -19.32947785509334082, 63.04547287423799418, 19.42212676744230393 ) ) ;
#1385 = DIRECTION ( 'NONE',  ( 1.000000000000000000, 6.033820786006286457E-17, -0.000000000000000000 ) ) ;
#1386 = CARTESIAN_POINT ( 'NONE',  ( -0.8179331680533127313, -5.301268757141564869, -5.926062401966621707 ) ) ;
#1387 = CARTESIAN_POINT ( 'NONE',  ( -73.62500000000008527, 79.99999999999987210, -1.530808498934183435E-15 ) ) ;
#1388 = ORIENTED_EDGE ( 'NONE', *, *, #7898, .F. ) ;
#1389 = CARTESIAN_POINT ( 'NONE',  ( -78.00000000000002842, 50.75735931288069480, 5.742644059037076865 ) ) ;
#1390 = CARTESIAN_POINT ( 'NONE',  ( -74.28125000000000000, 30.00000000000000355, -10.35533905932738108 ) ) ;
#1391 = CARTESIAN_POINT ( 'NONE',  ( -72.59375000409677625, 80.00000000000001421, -10.35533905932737753 ) ) ;
#1392 = CARTESIAN_POINT ( 'NONE',  ( -52.42856357389445066, 59.99999999999997158, -5.034386850915387018E-15 ) ) ;
#1393 = EDGE_LOOP ( 'NONE', ( #5631, #3625 ) ) ;
#1394 = CARTESIAN_POINT ( 'NONE',  ( -45.89008546996493720, 61.09306511264237827, -3.515648168893299896 ) ) ;
#1395 = DIRECTION ( 'NONE',  ( 1.000000000000000000, 6.033820786006286457E-17, 0.000000000000000000 ) ) ;
#1396 = DIRECTION ( 'NONE',  ( 0.000000000000000000, 1.000000000000000000, 0.000000000000000000 ) ) ;
#1397 = ORIENTED_EDGE ( 'NONE', *, *, #5431, .T. ) ;
#1398 = CARTESIAN_POINT ( 'NONE',  ( 20.45981033141799088, 75.95367107335623302, 6.713009951748246884 ) ) ;
#1399 = CARTESIAN_POINT ( 'NONE',  ( -0.4079457818577089112, 5.537975084925939484, -5.789399939901066716 ) ) ;
#1400 = ORIENTED_EDGE ( 'NONE', *, *, #2192, .F. ) ;
#1401 = FACE_OUTER_BOUND ( 'NONE', #8358, .T. ) ;
#1402 = EDGE_CURVE ( 'NONE', #6890, #9107, #1544, .T. ) ;
#1403 = CARTESIAN_POINT ( 'NONE',  ( -78.00000000000002842, 59.24264068711927678, 11.22792543327563131 ) ) ;
#1404 = CARTESIAN_POINT ( 'NONE',  ( -1.240525345857069306, 54.99835318325028055, 0.02617781847627572225 ) ) ;
#1405 = FILL_AREA_STYLE ('',( #5909 ) ) ;
#1406 = DIRECTION ( 'NONE',  ( 0.000000000000000000, 0.000000000000000000, 1.000000000000000000 ) ) ;
#1407 = VERTEX_POINT ( 'NONE', #3518 ) ;
#1408 = EDGE_CURVE ( 'NONE', #932, #11654, #10812, .T. ) ;
#1409 = CARTESIAN_POINT ( 'NONE',  ( 2.981862520314375153, 0.000000000000000000, -0.01270000000000047133 ) ) ;
#1410 = ADVANCED_FACE ( 'NONE', ( #5150 ), #2091, .T. ) ;
#1411 =( BOUNDED_SURFACE ( )  B_SPLINE_SURFACE ( 1, 2, ( 
 ( #9364, #7103, #10667, #8770, #1629, #6085, #3316, #8950, #7878, #725, #1514, #10729, #11566, #5178, #550, #4458, #6984, #4215, #1459, #6204, #11509, #3369, #10605, #2412, #9838, #9718, #8888, #2538, #8049, #614, #2596, #8111, #8833, #9661, #7046, #784, #2477, #11746, #4276, #6142, #9779, #5355, #5296, #7934, #6027, #1575, #7161, #5240, #667, #11691, #4338, #7988, #3430, #11627, #4398, #3495, #10785, #6264, #9895, #5123, #1689, #6927, #9006, #10557, #2357, #963, #10063, #3723, #5596, #10960, #9233, #7222, #54, #6431, #4682, #10907, #7452, #6560, #5526, #11080, #7277, #2826, #8279, #1020, #6492, #7387, #8334 ),
 ( #4571, #9952, #3550, #3610, #117, #1861, #3784, #8225, #9176, #4628, #2717, #1923, #10122, #2770, #5468, #2891, #6379, #10190, #11014, #4509, #1800, #1980, #10006, #5649, #9287, #1082, #9116, #4748, #8399, #10849, #2654, #6321, #1750, #5413, #9061, #838, #898, #8164, #11806, #2394, #3670, #7334, #8521, #9474, #6678, #1260, #9413, #11257, #6795, #10306, #1205, #10244, #1327, #4930, #6857, #2164, #3184, #1140, #3128, #5777, #3907, #4870, #10423, #5834, #9351, #2104, #3069, #1391, #2224, #5892, #3968, #304, #361, #422, #7515, #11136, #9535, #6616, #4028, #2041, #7571, #4084, #10481, #8586, #7744, #11198, #11320 ) ),
 .UNSPECIFIED., .F., .F., .T. ) 
 B_SPLINE_SURFACE_WITH_KNOTS ( ( 2, 2 ),
 ( 3, 2, 2, 2, 2, 2, 2, 2, 2, 2, 2, 2, 2, 2, 2, 2, 2, 2, 2, 2, 2, 2, 2, 2, 2, 2, 2, 2, 2, 2, 2, 2, 2, 2, 2, 2, 2, 2, 2, 2, 2, 2, 2, 3 ),
 ( 0.000000000000000000, 1.000000000000000000 ),
 ( 0.000000000000000000, 0.02083333333333333218, 0.04166666666666666435, 0.06250000000000000000, 0.08333333333333332871, 0.1041666666666666713, 0.1250000000000000000, 0.1458333333333333426, 0.1666666666666666574, 0.1875000000000000000, 0.2083333333333333426, 0.2291666666666666574, 0.2500000000000000000, 0.2708333333333333148, 0.2916666666666666852, 0.3125000000000000000, 0.3333333333333333148, 0.3541666666666666852, 0.3750000000000000000, 0.3958333333333333148, 0.4166666666666666852, 0.4375000000000000000, 0.4583333333333333148, 0.4791666666666666852, 0.5000000000000000000, 0.5208333333333333703, 0.5416666666666666297, 0.5625000000000000000, 0.5833333333333333703, 0.6041666666666666297, 0.6250000000000000000, 0.6458333333333333703, 0.6666666666666666297, 0.6875000000000000000, 0.7083333333333333703, 0.7291666666666666297, 0.7500000000000000000, 0.7708333333333333703, 0.7916666666666666297, 0.8125000000000000000, 0.8333333333333333703, 0.8541666666666666297, 0.8750000000000000000, 0.8888490476107191451 ),
 .UNSPECIFIED. ) 
 GEOMETRIC_REPRESENTATION_ITEM ( )  RATIONAL_B_SPLINE_SURFACE ( (
 ( 1.000000000000000000, 0.9238795325112867385, 1.000000000000000000, 0.9238795325112867385, 1.000000000000000000, 0.9238795325112867385, 1.000000000000000000, 0.9238795325112867385, 1.000000000000000000, 0.9238795325112867385, 1.000000000000000000, 0.9238795325112867385, 1.000000000000000000, 0.9238795325112867385, 1.000000000000000000, 0.9238795325112867385, 1.000000000000000000, 0.9238795325112867385, 1.000000000000000000, 0.9238795325112867385, 1.000000000000000000, 0.9238795325112867385, 1.000000000000000000, 0.9238795325112867385, 1.000000000000000000, 0.9238795325112867385, 1.000000000000000000, 0.9238795325112867385, 1.000000000000000000, 0.9238795325112867385, 1.000000000000000000, 0.9238795325112867385, 1.000000000000000000, 0.9238795325112867385, 1.000000000000000000, 0.9238795325112867385, 1.000000000000000000, 0.9238795325112867385, 1.000000000000000000, 0.9238795325112867385, 1.000000000000000000, 0.9238795325112867385, 1.000000000000000000, 0.9238795325112867385, 1.000000000000000000, 0.9238795325112867385, 1.000000000000000000, 0.9238795325112867385, 1.000000000000000000, 0.9238795325112867385, 1.000000000000000000, 0.9238795325112867385, 1.000000000000000000, 0.9238795325112867385, 1.000000000000000000, 0.9238795325112867385, 1.000000000000000000, 0.9238795325112867385, 1.000000000000000000, 0.9238795325112867385, 1.000000000000000000, 0.9238795325112867385, 1.000000000000000000, 0.9238795325112867385, 1.000000000000000000, 0.9238795325112867385, 1.000000000000000000, 0.9238795325112867385, 1.000000000000000000, 0.9238795325112867385, 1.000000000000000000, 0.9238795325112867385, 1.000000000000000000, 0.9238795325112867385, 1.000000000000000000, 0.9238795325112867385, 1.000000000000000000, 0.9238795325112867385, 1.000000000000000000, 0.9238795325112867385, 1.000000000000000000, 0.9238795325112867385, 1.000000000000000000, 0.9238795325112867385, 1.000000000000000000, 0.9493985930367334625, 0.9660721903170175207),
 ( 1.000000000000000000, 0.9238795325112867385, 1.000000000000000000, 0.9238795325112867385, 1.000000000000000000, 0.9238795325112867385, 1.000000000000000000, 0.9238795325112867385, 1.000000000000000000, 0.9238795325112867385, 1.000000000000000000, 0.9238795325112867385, 1.000000000000000000, 0.9238795325112867385, 1.000000000000000000, 0.9238795325112867385, 1.000000000000000000, 0.9238795325112867385, 1.000000000000000000, 0.9238795325112867385, 1.000000000000000000, 0.9238795325112867385, 1.000000000000000000, 0.9238795325112867385, 1.000000000000000000, 0.9238795325112867385, 1.000000000000000000, 0.9238795325112867385, 1.000000000000000000, 0.9238795325112867385, 1.000000000000000000, 0.9238795325112867385, 1.000000000000000000, 0.9238795325112867385, 1.000000000000000000, 0.9238795325112867385, 1.000000000000000000, 0.9238795325112867385, 1.000000000000000000, 0.9238795325112867385, 1.000000000000000000, 0.9238795325112867385, 1.000000000000000000, 0.9238795325112867385, 1.000000000000000000, 0.9238795325112867385, 1.000000000000000000, 0.9238795325112867385, 1.000000000000000000, 0.9238795325112867385, 1.000000000000000000, 0.9238795325112867385, 1.000000000000000000, 0.9238795325112867385, 1.000000000000000000, 0.9238795325112867385, 1.000000000000000000, 0.9238795325112867385, 1.000000000000000000, 0.9238795325112867385, 1.000000000000000000, 0.9238795325112867385, 1.000000000000000000, 0.9238795325112867385, 1.000000000000000000, 0.9238795325112867385, 1.000000000000000000, 0.9238795325112867385, 1.000000000000000000, 0.9238795325112867385, 1.000000000000000000, 0.9238795325112867385, 1.000000000000000000, 0.9238795325112867385, 1.000000000000000000, 0.9238795325112867385, 1.000000000000000000, 0.9238795325112867385, 1.000000000000000000, 0.9238795325112867385, 1.000000000000000000, 0.9238795325112867385, 1.000000000000000000, 0.9238795325112867385, 1.000000000000000000, 0.9493985930367334625, 0.9660721903170175207) ) ) 
 REPRESENTATION_ITEM ( '' )  SURFACE ( )  );
#1412 = CARTESIAN_POINT ( 'NONE',  ( -42.33720994522852266, 55.00043528610386545, -21.02753041772728437 ) ) ;
#1413 = ORIENTED_EDGE ( 'NONE', *, *, #6593, .F. ) ;
#1414 = CARTESIAN_POINT ( 'NONE',  ( 6.173066176615439105, 34.30768362678504957, 4.109395208432498947 ) ) ;
#1415 = CARTESIAN_POINT ( 'NONE',  ( -24.79373960380069164, 53.16908519469900085, 14.01800865919465799 ) ) ;
#1416 = DIRECTION ( 'NONE',  ( 0.000000000000000000, 0.000000000000000000, 1.000000000000000000 ) ) ;
#1417 = CARTESIAN_POINT ( 'NONE',  ( -78.00000000000002842, 46.51471862576140381, 8.485284746156354529 ) ) ;
#1418 = CARTESIAN_POINT ( 'NONE',  ( -78.12500000409677625, 55.00000000000000000, 24.99999999999999645 ) ) ;
#1419 = VERTEX_POINT ( 'NONE', #3468 ) ;
#1420 = CARTESIAN_POINT ( 'NONE',  ( -72.31250000000000000, 72.67766952966368876, -17.67766952966368876 ) ) ;
#1421 = DIRECTION ( 'NONE',  ( -1.000000000000000000, -0.000000000000000000, -0.000000000000000000 ) ) ;
#1422 =( NAMED_UNIT ( * ) PLANE_ANGLE_UNIT ( ) SI_UNIT ( $, .RADIAN. ) );
#1423 = LINE ( 'NONE', #460, #11019 ) ;
#1424 = CARTESIAN_POINT ( 'NONE',  ( -48.44321661921154032, 60.60981481080942501, -4.313990038473558108 ) ) ;
#1425 = ORIENTED_EDGE ( 'NONE', *, *, #4742, .T. ) ;
#1426 = CARTESIAN_POINT ( 'NONE',  ( -28.36397722366938012, 36.00052710555507218, 8.986026874162561739 ) ) ;
#1427 = CARTESIAN_POINT ( 'NONE',  ( 14.47760468889531182, 57.74566952947367326, 20.98118467575540436 ) ) ;
#1428 = CARTESIAN_POINT ( 'NONE',  ( -2.500000000000003553, 4.330127018922192761, 0.000000000000000000 ) ) ;
#1429 = CARTESIAN_POINT ( 'NONE',  ( -76.90625000204839523, 36.74823131438026280, 18.25176868561974786 ) ) ;
#1430 = ADVANCED_FACE ( 'NONE', ( #7134 ), #4393, .F. ) ;
#1431 = CARTESIAN_POINT ( 'NONE',  ( -4.637059203130386109, 66.15064323337712437, 22.37599513459590028 ) ) ;
#1432 = CARTESIAN_POINT ( 'NONE',  ( -75.12500000204838102, 29.18810118750000626, -10.69163855873949309 ) ) ;
#1433 = ORIENTED_EDGE ( 'NONE', *, *, #3169, .T. ) ;
#1434 = CARTESIAN_POINT ( 'NONE',  ( -75.03125000409677625, 44.64466094067262958, 25.00000000000001066 ) ) ;
#1435 = DIRECTION ( 'NONE',  ( -1.000000000000000000, 0.000000000000000000, 0.000000000000000000 ) ) ;
#1436 = DIRECTION ( 'NONE',  ( -1.000000000000000000, -6.033820786006286457E-17, -0.000000000000000000 ) ) ;
#1437 = CARTESIAN_POINT ( 'NONE',  ( -11.52239577449127061, 75.97627689174807131, -2.745668057393931161 ) ) ;
#1438 = CARTESIAN_POINT ( 'NONE',  ( -75.40625000000007105, 65.35533905932709331, -25.00000000000012790 ) ) ;
#1439 = CARTESIAN_POINT ( 'NONE',  ( -1.648146632869007089, -4.821944789745371551, -6.099999999999998757 ) ) ;
#1440 = STYLED_ITEM ( 'NONE', ( #5732 ), #4566 ) ;
#1441 = AXIS2_PLACEMENT_3D ( 'NONE', #1417, #1628, #5294 ) ;
#1442 = VERTEX_POINT ( 'NONE', #4653 ) ;
#1443 = CARTESIAN_POINT ( 'NONE',  ( -80.00000000000002842, 42.27207793864211283, 14.22792543327562775 ) ) ;
#1444 = CARTESIAN_POINT ( 'NONE',  ( -74.09375000000000000, 44.64466094067260826, -24.99999999999998934 ) ) ;
#1445 = DIRECTION ( 'NONE',  ( 9.813077866773612233E-16, -1.000000000000000000, -0.000000000000000000 ) ) ;
#1446 = ADVANCED_FACE ( 'NONE', ( #10935 ), #10312, .T. ) ;
#1447 = DIRECTION ( 'NONE',  ( 0.000000000000000000, 0.000000000000000000, -1.000000000000000000 ) ) ;
#1448 = ORIENTED_EDGE ( 'NONE', *, *, #2574, .T. ) ;
#1449 = CARTESIAN_POINT ( 'NONE',  ( -50.16689083095988622, 61.89286798645840548, 1.372268717346541989 ) ) ;
#1450 = CARTESIAN_POINT ( 'NONE',  ( -77.75000000000000000, 55.00000000000000000, 24.99999999999999645 ) ) ;
#1451 = ADVANCED_FACE ( 'NONE', ( #8251 ), #2684, .T. ) ;
#1452 = CARTESIAN_POINT ( 'NONE',  ( -4.182066831946700702, 3.358985280702823317, -5.926062401966626147 ) ) ;
#1453 = PRODUCT ( 'Table Clamp Lock Screw', 'Table Clamp Lock Screw', '', ( #9179 ) ) ;
#1454 = VECTOR ( 'NONE', #1644, 1000.000000000000000 ) ;
#1455 = ORIENTED_EDGE ( 'NONE', *, *, #2211, .F. ) ;
#1456 = CARTESIAN_POINT ( 'NONE',  ( 11.22402665386259280, 69.04425390357937431, -16.94073621750904124 ) ) ;
#1457 = CARTESIAN_POINT ( 'NONE',  ( -75.40625000204838102, 29.18810118750000271, 4.741568889096522788E-15 ) ) ;
#1458 = ORIENTED_EDGE ( 'NONE', *, *, #7447, .T. ) ;
#1459 = CARTESIAN_POINT ( 'NONE',  ( -77.65625000204839523, 73.25176868561975141, -18.25176868561974430 ) ) ;
#1460 = EDGE_CURVE ( 'NONE', #2849, #8906, #2855, .T. ) ;
#1461 = DIRECTION ( 'NONE',  ( 6.033820786006286457E-17, -1.000000000000000000, 0.000000000000000000 ) ) ;
#1462 = AXIS2_PLACEMENT_3D ( 'NONE', #6148, #7884, #6269 ) ;
#1463 = CARTESIAN_POINT ( 'NONE',  ( -75.87500000409677625, 55.00000000000000000, -24.99999999999999645 ) ) ;
#1464 = CARTESIAN_POINT ( 'NONE',  ( -16.87154951642690648, 55.00301719933347044, 0.003379411846644060982 ) ) ;
#1465 = DIRECTION ( 'NONE',  ( 0.000000000000000000, 0.000000000000000000, 1.000000000000000000 ) ) ;
#1466 = CARTESIAN_POINT ( 'NONE',  ( -75.00000000000004263, 33.65755212260173579, -14.43688233189822334 ) ) ;
#1467 = ORIENTED_EDGE ( 'NONE', *, *, #8813, .F. ) ;
#1468 = CARTESIAN_POINT ( 'NONE',  ( -78.00000000000002842, 50.75735931288069480, 11.22792543327563131 ) ) ;
#1469 = CARTESIAN_POINT ( 'NONE',  ( -36.14426256656389569, 36.63180902967581432, -10.58010824564746599 ) ) ;
#1470 = EDGE_LOOP ( 'NONE', ( #2824, #11364, #11751, #8308 ) ) ;
#1471 = CARTESIAN_POINT ( 'NONE',  ( -7.548092367965108629, 65.81078796322651669, -18.03704516092939869 ) ) ;
#1472 = CARTESIAN_POINT ( 'NONE',  ( -31.00186844413243392, 42.04798375885678752, 5.364520326994415278 ) ) ;
#1473 = CARTESIAN_POINT ( 'NONE',  ( 53.00000000000000000, 47.00000000000000711, 0.000000000000000000 ) ) ;
#1474 = AXIS2_PLACEMENT_3D ( 'NONE', #5522, #7565, #3064 ) ;
#1475 = AXIS2_PLACEMENT_3D ( 'NONE', #345, #4914, #2086 ) ;
#1476 = ORIENTED_EDGE ( 'NONE', *, *, #6323, .T. ) ;
#1477 = CARTESIAN_POINT ( 'NONE',  ( -77.75000000204839523, 80.81189881250001861, -10.69163855873949132 ) ) ;
#1478 = DIRECTION ( 'NONE',  ( 1.000000000000000000, 6.033820786006286457E-17, -0.000000000000000000 ) ) ;
#1479 =( BOUNDED_CURVE ( )  B_SPLINE_CURVE ( 2, ( #8361, #5801, #5616, #9435, #1223, #10269, #5552, #7412, #10146 ),
 .UNSPECIFIED., .F., .T. ) 
 B_SPLINE_CURVE_WITH_KNOTS ( ( 3, 2, 2, 2, 3 ),
 ( 0.1584082455038353654, 0.1782132311131151281, 0.1980182167223948908, 0.2178232023316745980, 0.2376281879409543607 ),
 .UNSPECIFIED. ) 
 CURVE ( )  GEOMETRIC_REPRESENTATION_ITEM ( )  RATIONAL_B_SPLINE_CURVE ( ( 1.000000000000020650, 0.9238795325112661994, 1.000000000000000000, 0.9238795325112868495, 1.000000000000000000, 0.9238795325112868495, 1.000000000000000000, 0.9238795325112363344, 1.000000000000050404 ) ) 
 REPRESENTATION_ITEM ( '' )  );
#1480 = CYLINDRICAL_SURFACE ( 'NONE', #355, 24.99999999999999645 ) ;
#1481 = AXIS2_PLACEMENT_3D ( 'NONE', #1029, #4878, #11267 ) ;
#1482 = DIRECTION ( 'NONE',  ( -9.813077866773612233E-16, 1.000000000000000000, 0.000000000000000000 ) ) ;
#1483 = CARTESIAN_POINT ( 'NONE',  ( -19.66652697884454781, 59.95698360088004364, 4.957362171560429687 ) ) ;
#1484 = ORIENTED_EDGE ( 'NONE', *, *, #3072, .T. ) ;
#1485 = EDGE_CURVE ( 'NONE', #4583, #10943, #11068, .T. ) ;
#1486 = CARTESIAN_POINT ( 'NONE',  ( -42.96936073659074395, 63.99245613053683712, -19.01383356661934343 ) ) ;
#1487 = DIRECTION ( 'NONE',  ( 1.000000000000000000, 0.000000000000000000, 0.000000000000000000 ) ) ;
#1488 = DIRECTION ( 'NONE',  ( -0.000000000000000000, -0.000000000000000000, -1.000000000000000000 ) ) ;
#1489 = CARTESIAN_POINT ( 'NONE',  ( -77.56250000204839523, 80.81189881250000440, -10.69163855873948954 ) ) ;
#1490 = CARTESIAN_POINT ( 'NONE',  ( 0.000000000000000000, 0.000000000000000000, -0.3851141460153411078 ) ) ;
#1491 = CARTESIAN_POINT ( 'NONE',  ( -73.62500000204842365, 29.18810118750000626, -10.69163855873949309 ) ) ;
#1492 = VERTEX_POINT ( 'NONE', #6350 ) ;
#1493 = CARTESIAN_POINT ( 'NONE',  ( -71.93750000409677625, 37.32233047033631124, 17.67766952966369232 ) ) ;
#1494 = CARTESIAN_POINT ( 'NONE',  ( -78.00000000000000000, 55.00000000000000000, 0.000000000000000000 ) ) ;
#1495 = FACE_BOUND ( 'NONE', #2402, .T. ) ;
#1496 = VECTOR ( 'NONE', #2822, 1000.000000000000000 ) ;
#1497 = CARTESIAN_POINT ( 'NONE',  ( 6.636022776496402820, 34.00797225689733239, 1.031222807066483504 ) ) ;
#1498 = CARTESIAN_POINT ( 'NONE',  ( -76.53125000204838102, 55.00000000000000000, -25.81189881249999729 ) ) ;
#1499 = CARTESIAN_POINT ( 'NONE',  ( -2.500000000000005773, -4.330127018922191873, -6.099999999999999645 ) ) ;
#1500 = DIRECTION ( 'NONE',  ( 0.000000000000000000, 1.000000000000000000, 0.000000000000000000 ) ) ;
#1501 = DIRECTION ( 'NONE',  ( 0.000000000000000000, 0.000000000000000000, 1.000000000000000000 ) ) ;
#1502 = CARTESIAN_POINT ( 'NONE',  ( -79.25000000204838102, 80.81189881250001861, -10.69163855873949132 ) ) ;
#1503 = DIRECTION ( 'NONE',  ( 0.000000000000000000, 0.000000000000000000, -1.000000000000000000 ) ) ;
#1504 = EDGE_LOOP ( 'NONE', ( #9141, #37, #8640, #10332 ) ) ;
#1505 = FACE_OUTER_BOUND ( 'NONE', #8291, .T. ) ;
#1506 = UNCERTAINTY_MEASURE_WITH_UNIT (LENGTH_MEASURE( 1.000000000000000082E-05 ), #11513, 'distance_accuracy_value', 'NONE');
#1507 = VERTEX_POINT ( 'NONE', #8306 ) ;
#1508 = CARTESIAN_POINT ( 'NONE',  ( -28.58294521375118791, 48.28461196395628718, 2.037989642863114348 ) ) ;
#1509 = CARTESIAN_POINT ( 'NONE',  ( -77.09375000000004263, 44.64466094067264379, -24.99999999999989697 ) ) ;
#1510 = FACE_BOUND ( 'NONE', #8213, .T. ) ;
#1511 = CARTESIAN_POINT ( 'NONE',  ( 21.62726510572514727, 76.92664994937649681, 1.832148689196935187 ) ) ;
#1512 = CARTESIAN_POINT ( 'NONE',  ( -74.93750000204838102, 65.69163855873948421, -25.81189881250000084 ) ) ;
#1513 = ORIENTED_EDGE ( 'NONE', *, *, #11196, .T. ) ;
#1514 = CARTESIAN_POINT ( 'NONE',  ( -78.40625000204839523, 36.74823131438026280, 18.25176868561974786 ) ) ;
#1515 = ADVANCED_FACE ( 'NONE', ( #3579 ), #5944, .F. ) ;
#1516 = DIRECTION ( 'NONE',  ( -1.000000000000000000, -0.000000000000000000, -0.000000000000000000 ) ) ;
#1517 = LINE ( 'NONE', #8835, #413 ) ;
#1518 = CARTESIAN_POINT ( 'NONE',  ( -18.61890672186335749, 55.00248007087589741, 0.008241009575747904742 ) ) ;
#1519 = VECTOR ( 'NONE', #8861, 1000.000000000000114 ) ;
#1520 = FILL_AREA_STYLE_COLOUR ( '', #663 ) ;
#1521 = VECTOR ( 'NONE', #6899, 1000.000000000000000 ) ;
#1522 = CARTESIAN_POINT ( 'NONE',  ( 0.000000000000000000, 0.000000000000000000, -1.239675197676287643 ) ) ;
#1523 = ORIENTED_EDGE ( 'NONE', *, *, #3095, .T. ) ;
#1524 = CARTESIAN_POINT ( 'NONE',  ( -3.346878500200761053, -3.841181488860384796, -0.05140428708383018575 ) ) ;
#1525 = EDGE_CURVE ( 'NONE', #1807, #3299, #8194, .T. ) ;
#1526 = CARTESIAN_POINT ( 'NONE',  ( -31.54809236465146682, 34.60179423563022283, 5.109615027512485419 ) ) ;
#1527 = ORIENTED_EDGE ( 'NONE', *, *, #9135, .T. ) ;
#1528 = CARTESIAN_POINT ( 'NONE',  ( -47.85572436634423354, 73.33185325676623734, -10.56518764769322516 ) ) ;
#1529 = CARTESIAN_POINT ( 'NONE',  ( -17.59538538452048684, 67.42122968706608788, 6.631564624215115167 ) ) ;
#1530 = CARTESIAN_POINT ( 'NONE',  ( -77.93750000204838102, 65.69163855873948421, -25.81189881250000440 ) ) ;
#1531 = ORIENTED_EDGE ( 'NONE', *, *, #9448, .F. ) ;
#1532 = CARTESIAN_POINT ( 'NONE',  ( -78.96875000204839523, 73.25176868561975141, 18.25176868561974075 ) ) ;
#1533 = CARTESIAN_POINT ( 'NONE',  ( 6.636022776496402820, 34.00797225689733239, 1.031222807066483504 ) ) ;
#1534 = ORIENTED_EDGE ( 'NONE', *, *, #3310, .T. ) ;
#1535 = VECTOR ( 'NONE', #192, 1000.000000000000000 ) ;
#1536 = CARTESIAN_POINT ( 'NONE',  ( -78.00000000000002842, 54.99999999999998579, 8.485284746156354529 ) ) ;
#1537 = DIRECTION ( 'NONE',  ( 0.000000000000000000, 0.000000000000000000, -1.000000000000000000 ) ) ;
#1538 = CARTESIAN_POINT ( 'NONE',  ( -53.50022385974906314, 61.89434742217085272, 1.372896053409885520 ) ) ;
#1539 = EDGE_LOOP ( 'NONE', ( #5443, #8996, #8262, #9 ) ) ;
#1540 = CARTESIAN_POINT ( 'NONE',  ( -57.27472358375123207, 61.14040963541170015, 20.20590277145669234 ) ) ;
#1541 = VECTOR ( 'NONE', #8889, 1000.000000000000000 ) ;
#1542 = FACE_OUTER_BOUND ( 'NONE', #491, .T. ) ;
#1543 = CARTESIAN_POINT ( 'NONE',  ( -1.734723475976807094E-14, -5.773502691896260863, -0.4465819873852071575 ) ) ;
#1544 = LINE ( 'NONE', #5211, #1519 ) ;
#1545 = CARTESIAN_POINT ( 'NONE',  ( -73.34375000204839523, 55.00000000000000000, -25.81189881249999729 ) ) ;
#1546 = AXIS2_PLACEMENT_3D ( 'NONE', #7939, #968, #5419 ) ;
#1547 = ADVANCED_FACE ( 'NONE', ( #1051 ), #3753, .T. ) ;
#1548 = ORIENTED_EDGE ( 'NONE', *, *, #5066, .F. ) ;
#1549 = CARTESIAN_POINT ( 'NONE',  ( -75.59375000409679046, 80.00000000000001421, -10.35533905932737753 ) ) ;
#1550 = LINE ( 'NONE', #6180, #928 ) ;
#1551 = CARTESIAN_POINT ( 'NONE',  ( -13.14429486149114013, 76.02373996650987920, 2.745652855075435994 ) ) ;
#1552 = CIRCLE ( 'NONE', #10724, 24.99999999999999645 ) ;
#1553 = ORIENTED_EDGE ( 'NONE', *, *, #2286, .F. ) ;
#1554 = AXIS2_PLACEMENT_3D ( 'NONE', #2158, #9281, #11250 ) ;
#1555 = CARTESIAN_POINT ( 'NONE',  ( -75.31250000204839523, 29.18810118750000626, -10.69163855873949132 ) ) ;
#1556 = CARTESIAN_POINT ( 'NONE',  ( -58.64797208933948269, 57.51009499518404056, 4.336531854824778875 ) ) ;
#1557 = EDGE_CURVE ( 'NONE', #2610, #4492, #10091, .T. ) ;
#1558 = CARTESIAN_POINT ( 'NONE',  ( -74.00000000000000000, 55.00000000000000000, -24.99999999999999645 ) ) ;
#1559 = CARTESIAN_POINT ( 'NONE',  ( -22.50647595179652072, 59.12487335784310005, 20.69694904210189179 ) ) ;
#1560 = CARTESIAN_POINT ( 'NONE',  ( 39.99999999999999289, 55.00000000000000000, 0.000000000000000000 ) ) ;
#1561 = AXIS2_PLACEMENT_3D ( 'NONE', #9701, #1608, #6009 ) ;
#1562 = CARTESIAN_POINT ( 'NONE',  ( -77.93750000204838102, 65.69163855873948421, -25.81189881250000440 ) ) ;
#1563 = AXIS2_PLACEMENT_3D ( 'NONE', #2359, #3142, #7048 ) ;
#1564 = DIRECTION ( 'NONE',  ( -1.000000000000000000, -0.000000000000000000, -0.000000000000000000 ) ) ;
#1565 = ORIENTED_EDGE ( 'NONE', *, *, #10552, .T. ) ;
#1566 = DIRECTION ( 'NONE',  ( -0.000000000000000000, -0.000000000000000000, -1.000000000000000000 ) ) ;
#1567 = ORIENTED_EDGE ( 'NONE', *, *, #9736, .T. ) ;
#1568 = CARTESIAN_POINT ( 'NONE',  ( -57.16684244878135246, 56.37008073134157371, 6.893775596464392308 ) ) ;
#1569 = CARTESIAN_POINT ( 'NONE',  ( -3.000000000000000000, 0.000000000000000000, -4.346257142857142597 ) ) ;
#1570 = CARTESIAN_POINT ( 'NONE',  ( -79.43750000204838102, 55.00000000000000000, -25.81189881249999729 ) ) ;
#1571 = CARTESIAN_POINT ( 'NONE',  ( -78.50000000000000000, 55.00000000000000000, -24.99999999999999645 ) ) ;
#1572 = CARTESIAN_POINT ( 'NONE',  ( 1.476596942546186009, 65.05810802274424987, 19.56659622200108473 ) ) ;
#1573 = CARTESIAN_POINT ( 'NONE',  ( 5.000000000000000888, 0.9828435001097617363, -6.056909652965543067 ) ) ;
#1574 = ORIENTED_EDGE ( 'NONE', *, *, #741, .F. ) ;
#1575 = CARTESIAN_POINT ( 'NONE',  ( -75.12500000204838102, 29.18810118750000626, -10.69163855873949309 ) ) ;
#1576 = DIRECTION ( 'NONE',  ( -1.000000000000000000, -0.000000000000000000, -0.000000000000000000 ) ) ;
#1577 = DIRECTION ( 'NONE',  ( -1.000000000000000000, -6.033820786006286457E-17, 0.000000000000000000 ) ) ;
#1578 = CARTESIAN_POINT ( 'NONE',  ( 18.24053854380704820, 55.00849189285069230, 0.02483751907359685318 ) ) ;
#1579 = CARTESIAN_POINT ( 'NONE',  ( -74.99999999999998579, 36.75304232195939136, 17.29401847480263754 ) ) ;
#1580 = EDGE_LOOP ( 'NONE', ( #1273, #4112 ) ) ;
#1581 = DIRECTION ( 'NONE',  ( -1.000000000000000000, -0.000000000000000000, -0.000000000000000000 ) ) ;
#1582 = LINE ( 'NONE', #1637, #9387 ) ;
#1583 = ORIENTED_EDGE ( 'NONE', *, *, #1316, .T. ) ;
#1584 = CARTESIAN_POINT ( 'NONE',  ( -51.60828739328132997, 76.01535744515140891, 2.059423361852914969 ) ) ;
#1585 = CARTESIAN_POINT ( 'NONE',  ( -52.59538850930821496, 69.01351387254386793, 1.373364761778438581 ) ) ;
#1586 = CARTESIAN_POINT ( 'NONE',  ( -78.96875000204839523, 73.25176868561975141, 18.25176868561974075 ) ) ;
#1587 = ORIENTED_EDGE ( 'NONE', *, *, #5073, .T. ) ;
#1588 = CARTESIAN_POINT ( 'NONE',  ( -76.81250000204838102, 29.18810118750000626, -10.69163855873949309 ) ) ;
#1589 = CARTESIAN_POINT ( 'NONE',  ( 5.737308841168996310, 34.06700459503902323, -2.059191599423306318 ) ) ;
#1590 = ORIENTED_EDGE ( 'NONE', *, *, #299, .T. ) ;
#1591 = DIRECTION ( 'NONE',  ( 0.000000000000000000, 0.000000000000000000, -1.000000000000000000 ) ) ;
#1592 = ADVANCED_FACE ( 'NONE', ( #7420 ), #9088, .F. ) ;
#1593 = CARTESIAN_POINT ( 'NONE',  ( 23.81438878217834088, 59.74505718300422075, 1.610512999816130497 ) ) ;
#1594 = CARTESIAN_POINT ( 'NONE',  ( -67.10978172608912473, 49.39091922923409328, 4.313686075943445886 ) ) ;
#1595 = ORIENTED_EDGE ( 'NONE', *, *, #7678, .F. ) ;
#1596 = CARTESIAN_POINT ( 'NONE',  ( -7.737413764666613680, 68.33402667507452577, -16.24506794676610610 ) ) ;
#1597 = LINE ( 'NONE', #9576, #4710 ) ;
#1598 = CARTESIAN_POINT ( 'NONE',  ( 2.074714256722481220, -4.575665857285988736, -0.01055556052339421194 ) ) ;
#1599 = CARTESIAN_POINT ( 'NONE',  ( -78.00000000000001421, 71.97056274847716395, -1.499996628082204797 ) ) ;
#1600 = AXIS2_PLACEMENT_3D ( 'NONE', #6174, #4367, #8018 ) ;
#1601 = CARTESIAN_POINT ( 'NONE',  ( 73.00000000000000000, 97.00000000000000000, -9.797174393178809880E-16 ) ) ;
#1602 = ORIENTED_EDGE ( 'NONE', *, *, #3934, .T. ) ;
#1603 = CARTESIAN_POINT ( 'NONE',  ( -72.21875000409676204, 65.35533905932737753, 24.99999999999999645 ) ) ;
#1604 = PLANE ( 'NONE',  #7645 ) ;
#1605 = LINE ( 'NONE', #5390, #2905 ) ;
#1606 = CARTESIAN_POINT ( 'NONE',  ( -37.18898618307433424, 44.43582214169357769, -18.32873044267784479 ) ) ;
#1607 = ORIENTED_EDGE ( 'NONE', *, *, #9016, .F. ) ;
#1608 = DIRECTION ( 'NONE',  ( -1.000000000000000000, -0.000000000000000000, -0.000000000000000000 ) ) ;
#1609 = DIRECTION ( 'NONE',  ( 1.000000000000000000, 0.000000000000000000, 0.000000000000000000 ) ) ;
#1610 = EDGE_CURVE ( 'NONE', #1730, #6548, #1829, .T. ) ;
#1611 = DIRECTION ( 'NONE',  ( 0.000000000000000000, 0.000000000000000000, 1.000000000000000000 ) ) ;
#1612 = CARTESIAN_POINT ( 'NONE',  ( 8.623112943508827399, 51.69526317675230587, 3.766397512801251235 ) ) ;
#1613 = CARTESIAN_POINT ( 'NONE',  ( 4.592054218142289201, 3.122278952918446038, -5.789399939901072933 ) ) ;
#1614 = CARTESIAN_POINT ( 'NONE',  ( -79.34375000204839523, 73.25176868561975141, -18.25176868561974430 ) ) ;
#1615 = DIRECTION ( 'NONE',  ( 0.000000000000000000, 0.000000000000000000, 1.000000000000000000 ) ) ;
#1616 = ORIENTED_EDGE ( 'NONE', *, *, #839, .T. ) ;
#1617 = DIRECTION ( 'NONE',  ( -1.000000000000000000, -0.000000000000000000, -0.000000000000000000 ) ) ;
#1618 = VERTEX_POINT ( 'NONE', #10216 ) ;
#1619 = ADVANCED_FACE ( 'NONE', ( #8369 ), #2009, .F. ) ;
#1620 = CARTESIAN_POINT ( 'NONE',  ( -42.00013555804697774, 57.68060557487371653, -6.472410377448052365 ) ) ;
#1621 = CARTESIAN_POINT ( 'NONE',  ( -7.511572993685809947E-16, -5.773502691896268857, -6.099999999999999645 ) ) ;
#1622 = DIRECTION ( 'NONE',  ( 0.000000000000000000, 1.000000000000000000, 0.000000000000000000 ) ) ;
#1623 =( GEOMETRIC_REPRESENTATION_CONTEXT ( 3 ) GLOBAL_UNCERTAINTY_ASSIGNED_CONTEXT ( ( #1506 ) ) GLOBAL_UNIT_ASSIGNED_CONTEXT ( ( #11513, #10610, #3437 ) ) REPRESENTATION_CONTEXT ( 'NONE', 'WORKASPACE' ) );
#1624 = CARTESIAN_POINT ( 'NONE',  ( 0.7390892720871951038, 65.01136756371364811, -19.59014205680648502 ) ) ;
#1625 = CARTESIAN_POINT ( 'NONE',  ( -74.84375000204839523, 73.25176868561975141, -18.25176868561974430 ) ) ;
#1626 = VERTEX_POINT ( 'NONE', #2920 ) ;
#1627 = EDGE_CURVE ( 'NONE', #306, #8424, #2291, .T. ) ;
#1628 = DIRECTION ( 'NONE',  ( -1.000000000000000000, -0.000000000000000000, -0.000000000000000000 ) ) ;
#1629 = CARTESIAN_POINT ( 'NONE',  ( -78.96875000204839523, 80.81189881250000440, -1.580522963032174394E-15 ) ) ;
#1630 = CARTESIAN_POINT ( 'NONE',  ( -15.00000000000000000, -30.00000000000000000, -10.00000000000000000 ) ) ;
#1631 = DIRECTION ( 'NONE',  ( 0.000000000000000000, -0.000000000000000000, 1.000000000000000000 ) ) ;
#1632 = CARTESIAN_POINT ( 'NONE',  ( -6.952240055115057160, 55.00666461818682507, -0.005444984560454538616 ) ) ;
#1633 = CARTESIAN_POINT ( 'NONE',  ( -74.99999999999992895, 32.96633592742742991, 12.31671744011198122 ) ) ;
#1634 = EDGE_LOOP ( 'NONE', ( #5518, #10881, #4927 ) ) ;
#1635 = CARTESIAN_POINT ( 'NONE',  ( -20.51396975634441944, 55.33168391584075607, 4.991693283627284039 ) ) ;
#1636 = APPLICATION_CONTEXT ( 'automotive_design' ) ;
#1637 = CARTESIAN_POINT ( 'NONE',  ( 46.99999999999999289, 58.53553390593273065, 3.535533905932731091 ) ) ;
#1638 = ORIENTED_EDGE ( 'NONE', *, *, #9937, .T. ) ;
#1639 = CARTESIAN_POINT ( 'NONE',  ( -50.18900491406688502, 75.97955728750814330, -2.745941717788443537 ) ) ;
#1640 = CARTESIAN_POINT ( 'NONE',  ( -75.68750000204838102, 44.30836144126053000, 25.81189881250000795 ) ) ;
#1641 = VECTOR ( 'NONE', #9613, 1000.000000000000000 ) ;
#1642 = ORIENTED_EDGE ( 'NONE', *, *, #1110, .F. ) ;
#1643 = CARTESIAN_POINT ( 'NONE',  ( -73.34375000204839523, 73.25176868561975141, -18.25176868561974430 ) ) ;
#1644 = DIRECTION ( 'NONE',  ( 0.8191520442889911324, 0.000000000000000000, 0.5735764363510470476 ) ) ;
#1645 = VECTOR ( 'NONE', #5602, 1000.000000000000000 ) ;
#1646 =( NAMED_UNIT ( * ) PLANE_ANGLE_UNIT ( ) SI_UNIT ( $, .RADIAN. ) );
#1647 = ORIENTED_EDGE ( 'NONE', *, *, #1808, .F. ) ;
#1648 = CARTESIAN_POINT ( 'NONE',  ( -80.00000000000001421, 63.48528137423857487, 3.371917795327861178E-06 ) ) ;
#1649 = CARTESIAN_POINT ( 'NONE',  ( 25.76190476190475565, 59.99999999999995026, 0.000000000000000000 ) ) ;
#1650 = CARTESIAN_POINT ( 'NONE',  ( -8.909737369126560225, 55.00301576531230552, -0.005174452243964258909 ) ) ;
#1651 = EDGE_LOOP ( 'NONE', ( #7480, #11260, #3913, #11469 ) ) ;
#1652 = CARTESIAN_POINT ( 'NONE',  ( -57.82750524721426189, 59.10997802641301035, 20.69196764327204008 ) ) ;
#1653 = VECTOR ( 'NONE', #2471, 1000.000000000000000 ) ;
#1654 = CARTESIAN_POINT ( 'NONE',  ( -34.72515708538001888, 34.82355399787605421, -6.128525890628534256 ) ) ;
#1655 = CARTESIAN_POINT ( 'NONE',  ( -2.500000000000000000, 3.061616997868383141E-16, -6.099999999999999645 ) ) ;
#1656 = VECTOR ( 'NONE', #285, 1000.000000000000000 ) ;
#1657 = DIRECTION ( 'NONE',  ( 0.000000000000000000, 0.000000000000000000, 1.000000000000000000 ) ) ;
#1658 = CARTESIAN_POINT ( 'NONE',  ( 3.000000000000000888, 3.673940397442060854E-16, -6.074599999999999334 ) ) ;
#1659 = VERTEX_POINT ( 'NONE', #3696 ) ;
#1660 = CARTESIAN_POINT ( 'NONE',  ( -77.00000000000000000, 55.00000000000000000, -24.99999999999999645 ) ) ;
#1661 = DIRECTION ( 'NONE',  ( 1.000000000000000000, 0.000000000000000000, 0.000000000000000000 ) ) ;
#1662 = CARTESIAN_POINT ( 'NONE',  ( -71.65625000409677625, 30.00000000000000355, -10.35533905932738108 ) ) ;
#1663 = CARTESIAN_POINT ( 'NONE',  ( -63.06671435217206323, 41.62111505249539078, 16.30162306856191989 ) ) ;
#1664 = VERTEX_POINT ( 'NONE', #1111 ) ;
#1665 = DIRECTION ( 'NONE',  ( -1.000000000000000000, 0.000000000000000000, 0.000000000000000000 ) ) ;
#1666 = AXIS2_PLACEMENT_3D ( 'NONE', #2364, #560, #2303 ) ;
#1667 = CARTESIAN_POINT ( 'NONE',  ( -61.36749305124384080, 55.33290285919624552, 4.999731327536861336 ) ) ;
#1668 = EDGE_CURVE ( 'NONE', #10082, #7521, #3824, .T. ) ;
#1669 = ORIENTED_EDGE ( 'NONE', *, *, #5875, .F. ) ;
#1670 = LINE ( 'NONE', #11732, #5906 ) ;
#1671 = CARTESIAN_POINT ( 'NONE',  ( 7.462649519108526697, 51.02641210518733317, 3.052499146972269983 ) ) ;
#1672 = CARTESIAN_POINT ( 'NONE',  ( -77.46875000204839523, 73.25176868561975141, 18.25176868561974075 ) ) ;
#1673 = CARTESIAN_POINT ( 'NONE',  ( 53.00000000000000000, 51.46446609406726935, -3.535533905932738197 ) ) ;
#1674 =( GEOMETRIC_REPRESENTATION_CONTEXT ( 3 ) GLOBAL_UNCERTAINTY_ASSIGNED_CONTEXT ( ( #5920 ) ) GLOBAL_UNIT_ASSIGNED_CONTEXT ( ( #6512, #6394, #916 ) ) REPRESENTATION_CONTEXT ( 'NONE', 'WORKASPACE' ) );
#1675 = VERTEX_POINT ( 'NONE', #9204 ) ;
#1676 = CYLINDRICAL_SURFACE ( 'NONE', #10532, 4.999999999999997335 ) ;
#1677 = EDGE_LOOP ( 'NONE', ( #5269, #4436, #10694, #736 ) ) ;
#1678 = CARTESIAN_POINT ( 'NONE',  ( 10.32208524953959916, 68.72075925444976008, 20.90353566436339960 ) ) ;
#1679 = CARTESIAN_POINT ( 'NONE',  ( -11.20624054502364864, 68.97545947489571461, -1.830994258430044930 ) ) ;
#1680 = DIRECTION ( 'NONE',  ( 1.000000000000000000, 0.000000000000000000, 0.000000000000000000 ) ) ;
#1681 = CARTESIAN_POINT ( 'NONE',  ( -15.00000000000000355, 5.000000000000000000, 30.00000000000000711 ) ) ;
#1682 = EDGE_CURVE ( 'NONE', #518, #6038, #6128, .T. ) ;
#1683 = AXIS2_PLACEMENT_3D ( 'NONE', #7917, #6012, #8752 ) ;
#1684 = EDGE_CURVE ( 'NONE', #5713, #1761, #6587, .T. ) ;
#1685 = EDGE_CURVE ( 'NONE', #10685, #1618, #2483, .T. ) ;
#1686 = PLANE ( 'NONE',  #11039 ) ;
#1687 = CARTESIAN_POINT ( 'NONE',  ( -80.00000000000002842, 42.27207793864211283, -5.742637315201479353 ) ) ;
#1688 = ORIENTED_EDGE ( 'NONE', *, *, #5113, .T. ) ;
#1689 = CARTESIAN_POINT ( 'NONE',  ( -73.71875000204839523, 29.18810118750000271, 4.741568889096522788E-15 ) ) ;
#1690 = B_SPLINE_CURVE_WITH_KNOTS ( 'NONE', 3,
 ( #6658, #6541, #11178, #2934 ),
 .UNSPECIFIED., .F., .F.,
 ( 4, 4 ),
 ( 2.380735200829041942E-07, 0.002921158011986710757 ),
 .UNSPECIFIED. ) ;
#1691 = DIRECTION ( 'NONE',  ( 0.000000000000000000, 1.000000000000000000, 0.000000000000000000 ) ) ;
#1692 = EDGE_CURVE ( 'NONE', #7395, #5447, #9503, .T. ) ;
#1693 = EDGE_CURVE ( 'NONE', #8038, #5411, #11291, .T. ) ;
#1694 = CYLINDRICAL_SURFACE ( 'NONE', #8455, 2.500000000000000000 ) ;
#1695 = CARTESIAN_POINT ( 'NONE',  ( -27.38106182849360337, 55.00820573016070369, -0.003135496005600075728 ) ) ;
#1696 = DIRECTION ( 'NONE',  ( 1.000000000000000000, 0.000000000000000000, 0.000000000000000000 ) ) ;
#1697 = CARTESIAN_POINT ( 'NONE',  ( -75.00000000000000000, 30.81391793133463608, -8.312227262611900258 ) ) ;
#1698 = ADVANCED_FACE ( 'NONE', ( #7540 ), #3997, .F. ) ;
#1699 = ORIENTED_EDGE ( 'NONE', *, *, #5066, .T. ) ;
#1700 = CARTESIAN_POINT ( 'NONE',  ( -11.37681534325029098, 59.99999999999997868, -0.1654421410166476147 ) ) ;
#1701 = CARTESIAN_POINT ( 'NONE',  ( -20.00000000000003197, -63.00000000000000000, 5.000000000000000000 ) ) ;
#1702 = EDGE_LOOP ( 'NONE', ( #4407, #4118 ) ) ;
#1703 = CARTESIAN_POINT ( 'NONE',  ( -20.66281120459677823, 63.04561409439726560, 19.42247919112690013 ) ) ;
#1704 = CARTESIAN_POINT ( 'NONE',  ( -75.12500000204838102, 44.30836144126050158, -25.81189881249999374 ) ) ;
#1705 = VECTOR ( 'NONE', #10638, 1000.000000000000000 ) ;
#1706 = VERTEX_POINT ( 'NONE', #5807 ) ;
#1707 = CARTESIAN_POINT ( 'NONE',  ( -74.28125000204838102, 55.00000000000000000, 25.81189881249999729 ) ) ;
#1708 = CARTESIAN_POINT ( 'NONE',  ( 0.000000000000000000, -17.82799999999998875, 0.000000000000000000 ) ) ;
#1709 = VERTEX_POINT ( 'NONE', #1175 ) ;
#1710 = DIRECTION ( 'NONE',  ( -1.000000000000000000, -0.000000000000000000, -0.000000000000000000 ) ) ;
#1711 = AXIS2_PLACEMENT_3D ( 'NONE', #5682, #148, #5558 ) ;
#1712 = CARTESIAN_POINT ( 'NONE',  ( 7.290226732917977515, 50.00000000000001421, 0.1647554015558948537 ) ) ;
#1713 = CARTESIAN_POINT ( 'NONE',  ( -4.426057251632187217, 54.99526716342594312, -0.01575941339944971972 ) ) ;
#1714 = AXIS2_PLACEMENT_3D ( 'NONE', #6464, #754, #11720 ) ;
#1715 = VERTEX_POINT ( 'NONE', #1418 ) ;
#1716 = CARTESIAN_POINT ( 'NONE',  ( 3.030639393851187524, 35.98666035303370592, -8.992230872156422805 ) ) ;
#1717 = CARTESIAN_POINT ( 'NONE',  ( -31.26269038945179446, 34.87416470039633509, 6.107602927758665423 ) ) ;
#1718 = B_SPLINE_CURVE_WITH_KNOTS ( 'NONE', 3,
 ( #9763, #3242, #4139, #9650 ),
 .UNSPECIFIED., .F., .F.,
 ( 4, 4 ),
 ( 2.380735200850890892E-07, 0.002921158011986708155 ),
 .UNSPECIFIED. ) ;
#1719 = CARTESIAN_POINT ( 'NONE',  ( -80.00000000000002842, 42.27207793864211283, 2.742644059037075976 ) ) ;
#1720 = CARTESIAN_POINT ( 'NONE',  ( 0.000000000000000000, 0.000000000000000000, -5.724496230895143256 ) ) ;
#1721 = CARTESIAN_POINT ( 'NONE',  ( 2.500000000000000000, 0.000000000000000000, -5.560532340533429263 ) ) ;
#1722 = ORIENTED_EDGE ( 'NONE', *, *, #1915, .T. ) ;
#1723 = DIRECTION ( 'NONE',  ( -0.000000000000000000, -0.000000000000000000, -1.000000000000000000 ) ) ;
#1724 = CARTESIAN_POINT ( 'NONE',  ( -78.00000000000001421, 59.24264068711928388, -12.72791868944003824 ) ) ;
#1725 = DIRECTION ( 'NONE',  ( 0.000000000000000000, 0.000000000000000000, -1.000000000000000000 ) ) ;
#1726 = ORIENTED_EDGE ( 'NONE', *, *, #10309, .T. ) ;
#1727 = DIRECTION ( 'NONE',  ( 0.000000000000000000, 1.000000000000000000, 0.000000000000000000 ) ) ;
#1728 = AXIS2_PLACEMENT_3D ( 'NONE', #11510, #9719, #5357 ) ;
#1729 = FACE_OUTER_BOUND ( 'NONE', #10500, .T. ) ;
#1730 = VERTEX_POINT ( 'NONE', #5989 ) ;
#1731 = EDGE_CURVE ( 'NONE', #1492, #6194, #6507, .T. ) ;
#1732 = DIRECTION ( 'NONE',  ( -1.000000000000000000, 0.000000000000000000, 0.000000000000000000 ) ) ;
#1733 = AXIS2_PLACEMENT_3D ( 'NONE', #11841, #4666, #2755 ) ;
#1734 = CARTESIAN_POINT ( 'NONE',  ( 53.00000000000000000, 55.00000000000000000, -6.000000000000000000 ) ) ;
#1735 = CARTESIAN_POINT ( 'NONE',  ( -75.68750000204838102, 44.30836144126053000, 25.81189881250000795 ) ) ;
#1736 = CARTESIAN_POINT ( 'NONE',  ( -78.68750000204838102, 44.30836144126053000, 25.81189881250000795 ) ) ;
#1737 = ORIENTED_EDGE ( 'NONE', *, *, #1076, .F. ) ;
#1738 = CARTESIAN_POINT ( 'NONE',  ( -78.31250000204839523, 29.18810118750000981, 10.69163855873950020 ) ) ;
#1739 = AXIS2_PLACEMENT_3D ( 'NONE', #8826, #718, #6918 ) ;
#1740 = ORIENTED_EDGE ( 'NONE', *, *, #6906, .F. ) ;
#1741 = CARTESIAN_POINT ( 'NONE',  ( -1.457434152866251775, 54.34000425242091126, -4.958991060964934583 ) ) ;
#1742 = CARTESIAN_POINT ( 'NONE',  ( -25.20616590903865628, 46.41268961681102212, 11.17697077816622020 ) ) ;
#1743 = CARTESIAN_POINT ( 'NONE',  ( -76.43750000204839523, 44.30836144126049447, -25.81189881249999019 ) ) ;
#1744 = LINE ( 'NONE', #6258, #1080 ) ;
#1745 = CARTESIAN_POINT ( 'NONE',  ( 2.500000000000005773, 4.330127018922190985, 0.000000000000000000 ) ) ;
#1746 = AXIS2_PLACEMENT_3D ( 'NONE', #8986, #8142, #5448 ) ;
#1747 = VERTEX_POINT ( 'NONE', #454 ) ;
#1748 = PRODUCT ( 'Threaded Front Retaining Ring Collar', 'Threaded Front Retaining Ring Collar', '', ( #7457 ) ) ;
#1749 = FACE_OUTER_BOUND ( 'NONE', #5704, .T. ) ;
#1750 = CARTESIAN_POINT ( 'NONE',  ( -75.87500000409677625, 55.00000000000000000, -24.99999999999999645 ) ) ;
#1751 = DIRECTION ( 'NONE',  ( -1.000000000000000000, -0.000000000000000000, -0.000000000000000000 ) ) ;
#1752 = DIRECTION ( 'NONE',  ( -1.000000000000000000, 3.552713678800500929E-15, 0.000000000000000000 ) ) ;
#1753 = CARTESIAN_POINT ( 'NONE',  ( -26.50353529629213867, 55.00548998525069067, -0.001986402032320984824 ) ) ;
#1754 = CARTESIAN_POINT ( 'NONE',  ( -13.89602465295604539, 70.84623132619663011, -15.29986294999528695 ) ) ;
#1755 = CARTESIAN_POINT ( 'NONE',  ( -22.46041777029512332, 53.70875712283432790, 4.841299448188346233 ) ) ;
#1756 = ADVANCED_FACE ( 'NONE', ( #271 ), #4960, .T. ) ;
#1757 = DIRECTION ( 'NONE',  ( -1.000000000000000000, -0.000000000000000000, -0.000000000000000000 ) ) ;
#1758 = ORIENTED_EDGE ( 'NONE', *, *, #11718, .F. ) ;
#1759 = CARTESIAN_POINT ( 'NONE',  ( -60.03167053577592327, 56.03207409872247524, 20.99365918962282862 ) ) ;
#1760 = CARTESIAN_POINT ( 'NONE',  ( -76.25000000204838102, 65.69163855873948421, -25.81189881250000440 ) ) ;
#1761 = VERTEX_POINT ( 'NONE', #10395 ) ;
#1762 = CARTESIAN_POINT ( 'NONE',  ( -80.00000000000001421, 67.72792206135787296, 5.742644059037073312 ) ) ;
#1763 = CARTESIAN_POINT ( 'NONE',  ( -7.662811188708723797, 69.86483622371564195, -14.86557385339502169 ) ) ;
#1764 =( NAMED_UNIT ( * ) PLANE_ANGLE_UNIT ( ) SI_UNIT ( $, .RADIAN. ) );
#1765 = EDGE_CURVE ( 'NONE', #1312, #11779, #8616, .T. ) ;
#1766 = B_SPLINE_CURVE_WITH_KNOTS ( 'NONE', 3,
 ( #126, #3791, #7460, #2898, #6566, #10195 ),
 .UNSPECIFIED., .F., .F.,
 ( 4, 2, 4 ),
 ( 0.008070708573309213693, 0.009531758523483285783, 0.01099280847365735614 ),
 .UNSPECIFIED. ) ;
#1767 = ORIENTED_EDGE ( 'NONE', *, *, #299, .F. ) ;
#1768 = CYLINDRICAL_SURFACE ( 'NONE', #9732, 1.500000000000001332 ) ;
#1769 = CARTESIAN_POINT ( 'NONE',  ( -65.16650212331052217, 51.09201045536845953, 5.853437054489593727 ) ) ;
#1770 = VERTEX_POINT ( 'NONE', #2977 ) ;
#1771 = CARTESIAN_POINT ( 'NONE',  ( -59.88037020503378471, 51.91452991566635689, 20.80113349088246011 ) ) ;
#1772 = CARTESIAN_POINT ( 'NONE',  ( -36.85572911278101316, 38.22258139949027367, -12.89445763391127464 ) ) ;
#1773 = CARTESIAN_POINT ( 'NONE',  ( -80.00000000000001421, 54.99999999999999289, -18.47055937655931501 ) ) ;
#1774 = DIRECTION ( 'NONE',  ( -1.000000000000000000, -0.000000000000000000, -0.000000000000000000 ) ) ;
#1775 = LINE ( 'NONE', #10873, #8415 ) ;
#1776 = VERTEX_POINT ( 'NONE', #10450 ) ;
#1777 = CARTESIAN_POINT ( 'NONE',  ( -75.00000000000000000, 55.00000000000000000, 29.00000000000000355 ) ) ;
#1778 = CARTESIAN_POINT ( 'NONE',  ( -46.82983832526868184, 55.00115022211477367, -0.002242098181359713800 ) ) ;
#1779 = CARTESIAN_POINT ( 'NONE',  ( -57.84573968844613034, 55.33154914686375037, 4.999987675084161864 ) ) ;
#1780 = ORIENTED_EDGE ( 'NONE', *, *, #7542, .T. ) ;
#1781 = CARTESIAN_POINT ( 'NONE',  ( -77.75000000000000000, 55.00000000000000000, 24.99999999999999645 ) ) ;
#1782 = CARTESIAN_POINT ( 'NONE',  ( -70.31421248054985540, 50.03279511399161095, 0.6584628854196864500 ) ) ;
#1783 = ORIENTED_EDGE ( 'NONE', *, *, #9045, .T. ) ;
#1784 = ADVANCED_FACE ( 'NONE', ( #2313 ), #368, .F. ) ;
#1785 = LINE ( 'NONE', #6246, #5721 ) ;
#1786 = CARTESIAN_POINT ( 'NONE',  ( 0.000000000000000000, 0.000000000000000000, 0.000000000000000000 ) ) ;
#1787 = PLANE ( 'NONE',  #11606 ) ;
#1788 = CARTESIAN_POINT ( 'NONE',  ( -72.21875000204838102, 36.74823131438024859, -18.25176868561973720 ) ) ;
#1789 = CARTESIAN_POINT ( 'NONE',  ( -77.28125000204838102, 55.00000000000000000, 25.81189881249999729 ) ) ;
#1790 = VERTEX_POINT ( 'NONE', #5026 ) ;
#1791 = CARTESIAN_POINT ( 'NONE',  ( 36.99999999999999289, 64.99999999999998579, 0.000000000000000000 ) ) ;
#1792 = ORIENTED_EDGE ( 'NONE', *, *, #10967, .T. ) ;
#1793 = CARTESIAN_POINT ( 'NONE',  ( -1.625240267017640655E-20, 65.42943686846950868, 22.72062601704910634 ) ) ;
#1794 = CARTESIAN_POINT ( 'NONE',  ( 5.788533022989986065, 41.13062614362130631, -2.057011258941260134 ) ) ;
#1795 = CARTESIAN_POINT ( 'NONE',  ( -74.99999999999998579, 39.36515909056227258, -20.53791299142421067 ) ) ;
#1796 = CARTESIAN_POINT ( 'NONE',  ( -77.28125000409677625, 65.35533905932743437, -24.99999999999994671 ) ) ;
#1797 = CARTESIAN_POINT ( 'NONE',  ( -77.84374999999997158, 65.35533905932209109, 25.00000000000518341 ) ) ;
#1798 = VERTEX_POINT ( 'NONE', #6880 ) ;
#1799 = EDGE_CURVE ( 'NONE', #5071, #8389, #2191, .T. ) ;
#1800 = CARTESIAN_POINT ( 'NONE',  ( -77.00000000409677625, 80.00000000000000000, -1.530808498934191324E-15 ) ) ;
#1801 = CARTESIAN_POINT ( 'NONE',  ( 0.000000000000000000, 0.000000000000000000, -6.099999999999999645 ) ) ;
#1802 =( BOUNDED_CURVE ( )  B_SPLINE_CURVE ( 2, ( #6603, #10230, #3115, #523, #6781, #10464, #5149, #4975, #3286, #1374, #6000, #4184, #5037, #2208, #2264, #10410, #5877, #8683, #8801, #1489, #580, #9634, #4246, #5937, #466, #4123, #1429, #11361, #10580, #7906, #8626, #6955, #6838, #9692, #9517, #7786, #5092, #2381, #6056, #11535, #6894, #11415, #1309, #408, #7670, #11305, #4073, #7730, #7846, #9578, #3170, #3226, #10522, #2330, #8740, #11474, #7531, #384, #8359, #8607, #261, #3029, #6697, #11098, #6515, #3804, #2913, #6759, #4765, #2125, #1041, #10267, #2065, #3092, #5736, #1284, #8421, #11279, #10328, #205, #9253, #2182, #8485, #5799, #4707, #5853, #8540 ),
 .UNSPECIFIED., .F., .T. ) 
 B_SPLINE_CURVE_WITH_KNOTS ( ( 3, 2, 2, 2, 2, 2, 2, 2, 2, 2, 2, 2, 2, 2, 2, 2, 2, 2, 2, 2, 2, 2, 2, 2, 2, 2, 2, 2, 2, 2, 2, 2, 2, 2, 2, 2, 2, 2, 2, 2, 2, 2, 2, 3 ),
 ( 0.000000000000000000, 0.02083333333333333218, 0.04166666666666666435, 0.06250000000000000000, 0.08333333333333332871, 0.1041666666666666713, 0.1250000000000000000, 0.1458333333333333148, 0.1666666666666666574, 0.1874999999999999722, 0.2083333333333333426, 0.2291666666666666852, 0.2500000000000000000, 0.2708333333333333148, 0.2916666666666666297, 0.3125000000000000000, 0.3333333333333333148, 0.3541666666666666852, 0.3749999999999999445, 0.3958333333333333148, 0.4166666666666666852, 0.4375000000000000000, 0.4583333333333333703, 0.4791666666666666852, 0.5000000000000000000, 0.5208333333333333703, 0.5416666666666666297, 0.5625000000000000000, 0.5833333333333332593, 0.6041666666666666297, 0.6250000000000000000, 0.6458333333333333703, 0.6666666666666666297, 0.6875000000000000000, 0.7083333333333333703, 0.7291666666666666297, 0.7499999999999998890, 0.7708333333333333703, 0.7916666666666666297, 0.8125000000000000000, 0.8333333333333333703, 0.8541666666666666297, 0.8750000000000000000, 0.8888490476107191451 ),
 .UNSPECIFIED. ) 
 CURVE ( )  GEOMETRIC_REPRESENTATION_ITEM ( )  RATIONAL_B_SPLINE_CURVE ( ( 1.000000000000000000, 0.9238795325112867385, 1.000000000000000000, 0.9238795325112867385, 1.000000000000000000, 0.9238795325112867385, 1.000000000000000000, 0.9238795325112867385, 1.000000000000000000, 0.9238795325112867385, 1.000000000000000000, 0.9238795325112867385, 1.000000000000000000, 0.9238795325112867385, 1.000000000000000000, 0.9238795325112867385, 1.000000000000000000, 0.9238795325112867385, 1.000000000000000000, 0.9238795325112867385, 1.000000000000000000, 0.9238795325112867385, 1.000000000000000000, 0.9238795325112867385, 1.000000000000000000, 0.9238795325112867385, 1.000000000000000000, 0.9238795325112867385, 1.000000000000000000, 0.9238795325112867385, 1.000000000000000000, 0.9238795325112867385, 1.000000000000000000, 0.9238795325112867385, 1.000000000000000000, 0.9238795325112867385, 1.000000000000000000, 0.9238795325112867385, 1.000000000000000000, 0.9238795325112867385, 1.000000000000000000, 0.9238795325112867385, 1.000000000000000000, 0.9238795325112867385, 1.000000000000000000, 0.9238795325112867385, 1.000000000000000000, 0.9238795325112867385, 1.000000000000000000, 0.9238795325112867385, 1.000000000000000000, 0.9238795325112867385, 1.000000000000000000, 0.9238795325112867385, 1.000000000000000000, 0.9238795325112867385, 1.000000000000000000, 0.9238795325112867385, 1.000000000000000000, 0.9238795325112867385, 1.000000000000000000, 0.9238795325112867385, 1.000000000000000000, 0.9238795325112867385, 1.000000000000000000, 0.9238795325112867385, 1.000000000000000000, 0.9238795325112867385, 1.000000000000000000, 0.9238795325112867385, 1.000000000000000000, 0.9238795325112867385, 1.000000000000000000, 0.9238795325112867385, 1.000000000000000000, 0.9238795325112867385, 1.000000000000000000, 0.9238795325112867385, 1.000000000000000000, 0.9238795325112867385, 1.000000000000000000, 0.9238795325112867385, 1.000000000000000000, 0.9238795325112867385, 1.000000000000000000, 0.9493985930367334625, 0.9660721903170175207 ) ) 
 REPRESENTATION_ITEM ( '' )  );
#1803 = CARTESIAN_POINT ( 'NONE',  ( -64.24754237443872285, 55.03769318549124279, -0.006317726105072558364 ) ) ;
#1804 = ITEM_DEFINED_TRANSFORMATION ( 'NONE', 'NONE', #6419,  #4738 ) ;
#1805 = CARTESIAN_POINT ( 'NONE',  ( -12.86143404212990227, 70.11511422732331766, -16.01369128662254582 ) ) ;
#1806 = CARTESIAN_POINT ( 'NONE',  ( -10.01312846213127905, 59.83883587255158432, -1.300640683813629295 ) ) ;
#1807 = VERTEX_POINT ( 'NONE', #395 ) ;
#1808 = EDGE_CURVE ( 'NONE', #3357, #11411, #2251, .T. ) ;
#1809 = CARTESIAN_POINT ( 'NONE',  ( -69.52691976458234535, 34.01892180236649921, 2.749684864678113794 ) ) ;
#1810 = VERTEX_POINT ( 'NONE', #4063 ) ;
#1811 = CARTESIAN_POINT ( 'NONE',  ( 4.636023424558444184, 34.00634798409771520, 1.031279783234476222 ) ) ;
#1812 = CARTESIAN_POINT ( 'NONE',  ( -74.00000000204839523, 29.18810118750000981, 10.69163855873950020 ) ) ;
#1813 = ORIENTED_EDGE ( 'NONE', *, *, #2839, .T. ) ;
#1814 = CARTESIAN_POINT ( 'NONE',  ( -75.31250000204839523, 29.18810118750000626, -10.69163855873949309 ) ) ;
#1815 = CARTESIAN_POINT ( 'NONE',  ( -10.81092923698156838, 75.47407628921179423, -5.508885182882011122 ) ) ;
#1816 = FILL_AREA_STYLE_COLOUR ( '', #8758 ) ;
#1817 = VERTEX_POINT ( 'NONE', #216 ) ;
#1818 = DIRECTION ( 'NONE',  ( 0.000000000000000000, 0.000000000000000000, 1.000000000000000000 ) ) ;
#1819 = ADVANCED_FACE ( 'NONE', ( #9566 ), #7720, .F. ) ;
#1820 = CARTESIAN_POINT ( 'NONE',  ( -11.82983844552040686, 55.00192051767528767, -0.001631283583225531103 ) ) ;
#1821 = VECTOR ( 'NONE', #2498, 1000.000000000000114 ) ;
#1822 = EDGE_LOOP ( 'NONE', ( #6558, #2902 ) ) ;
#1823 = CARTESIAN_POINT ( 'NONE',  ( -31.07074709816078695, 34.08442161144734683, 2.058417023654369071 ) ) ;
#1824 = EDGE_CURVE ( 'NONE', #7013, #10196, #8656, .T. ) ;
#1825 = CARTESIAN_POINT ( 'NONE',  ( -31.54809236465146682, 34.60179423563022283, 5.109615027512485419 ) ) ;
#1826 =( NAMED_UNIT ( * ) SI_UNIT ( $, .STERADIAN. ) SOLID_ANGLE_UNIT ( ) );
#1827 = FACE_OUTER_BOUND ( 'NONE', #3118, .T. ) ;
#1828 = VECTOR ( 'NONE', #11433, 1000.000000000000000 ) ;
#1829 = LINE ( 'NONE', #7306, #10505 ) ;
#1830 = DIRECTION ( 'NONE',  ( 0.000000000000000000, 0.000000000000000000, 1.000000000000000000 ) ) ;
#1831 = VERTEX_POINT ( 'NONE', #3653 ) ;
#1832 = CARTESIAN_POINT ( 'NONE',  ( -76.90625000000005684, 65.35533905932732068, -24.99999999999990052 ) ) ;
#1833 = CARTESIAN_POINT ( 'NONE',  ( -22.61890542003328619, 55.00133982146918044, 0.005189527613788253065 ) ) ;
#1834 = CARTESIAN_POINT ( 'NONE',  ( -32.95459766285684822, 50.50504115442574005, -2.214447714617367335 ) ) ;
#1835 = CONICAL_SURFACE ( 'NONE', #4136, 4.000000000000003553, 0.05235987755983000091 ) ;
#1836 = DIRECTION ( 'NONE',  ( -1.000000000000000000, 0.000000000000000000, 0.000000000000000000 ) ) ;
#1837 = PRODUCT_DEFINITION_SHAPE ( 'NONE', 'NONE',  #133 ) ;
#1838 = EDGE_CURVE ( 'NONE', #8743, #818, #1897, .T. ) ;
#1839 = AXIS2_PLACEMENT_3D ( 'NONE', #10418, #6010, #4133 ) ;
#1840 = FACE_BOUND ( 'NONE', #1900, .T. ) ;
#1841 = ORIENTED_EDGE ( 'NONE', *, *, #10879, .T. ) ;
#1842 = LINE ( 'NONE', #8146, #4176 ) ;
#1843 = DIRECTION ( 'NONE',  ( 6.033820786006286457E-17, -1.000000000000000000, 0.000000000000000000 ) ) ;
#1844 = CARTESIAN_POINT ( 'NONE',  ( 13.68354351360180132, 55.65895967216258811, 4.967044982674917009 ) ) ;
#1845 = CARTESIAN_POINT ( 'NONE',  ( -10.31596542140328587, 68.71721060802151726, -20.90586008767603587 ) ) ;
#1846 = CARTESIAN_POINT ( 'NONE',  ( -75.68750000204838102, 44.30836144126053000, 25.81189881250000795 ) ) ;
#1847 = ORIENTED_EDGE ( 'NONE', *, *, #9016, .T. ) ;
#1848 = VECTOR ( 'NONE', #8597, 1000.000000000000000 ) ;
#1849 = CARTESIAN_POINT ( 'NONE',  ( -79.25000000204838102, 65.69163855873948421, -25.81189881250000440 ) ) ;
#1850 = VERTEX_POINT ( 'NONE', #4609 ) ;
#1851 = DIRECTION ( 'NONE',  ( -1.000000000000000000, -0.000000000000000000, -0.000000000000000000 ) ) ;
#1852 = AXIS2_PLACEMENT_3D ( 'NONE', #2150, #8566, #3835 ) ;
#1853 = CARTESIAN_POINT ( 'NONE',  ( 8.404614611173400363, 41.52310116625425707, 4.095790913453249082 ) ) ;
#1854 = CARTESIAN_POINT ( 'NONE',  ( -79.34375000204839523, 55.00000000000000000, -25.81189881249999729 ) ) ;
#1855 = CARTESIAN_POINT ( 'NONE',  ( -75.00000000000000000, 80.22492272376648259, -0.3963795942728437494 ) ) ;
#1856 = DIRECTION ( 'NONE',  ( -0.000000000000000000, -1.000000000000000000, -0.000000000000000000 ) ) ;
#1857 = CIRCLE ( 'NONE', #7994, 1.500000000000001332 ) ;
#1858 = AXIS2_PLACEMENT_3D ( 'NONE', #4634, #7112, #10914 ) ;
#1859 = EDGE_LOOP ( 'NONE', ( #8569, #2807, #7885, #8102 ) ) ;
#1860 = LINE ( 'NONE', #9232, #10684 ) ;
#1861 = CARTESIAN_POINT ( 'NONE',  ( -78.40625000409677625, 80.00000000000001421, 10.35533905932737397 ) ) ;
#1862 = DIRECTION ( 'NONE',  ( 1.000000000000000000, 0.000000000000000000, 0.000000000000000000 ) ) ;
#1863 = APPLICATION_CONTEXT ( 'automotive_design' ) ;
#1864 = CARTESIAN_POINT ( 'NONE',  ( -62.09272923114016862, 55.00758854939876841, -0.01093042735399621553 ) ) ;
#1865 = DIRECTION ( 'NONE',  ( 0.000000000000000000, 0.000000000000000000, 1.000000000000000000 ) ) ;
#1866 = CARTESIAN_POINT ( 'NONE',  ( -20.07101753429484248, 75.63268020737004349, 7.663897408568258740 ) ) ;
#1867 = CARTESIAN_POINT ( 'NONE',  ( -26.34413835852909713, 51.02730822250849485, 3.053792540648594844 ) ) ;
#1868 = EDGE_LOOP ( 'NONE', ( #979, #6937 ) ) ;
#1869 = CARTESIAN_POINT ( 'NONE',  ( -74.00000000000000000, 55.00000000000000000, -24.99999999999999645 ) ) ;
#1870 = EDGE_LOOP ( 'NONE', ( #218, #5857, #11767, #5435 ) ) ;
#1871 = EDGE_CURVE ( 'NONE', #6614, #8495, #10170, .T. ) ;
#1872 = CARTESIAN_POINT ( 'NONE',  ( 19.14436220527237253, 71.77763100192429135, 12.89423484158165500 ) ) ;
#1873 = CARTESIAN_POINT ( 'NONE',  ( -77.84375000204839523, 55.00000000000000000, -25.81189881249999729 ) ) ;
#1874 = VERTEX_POINT ( 'NONE', #2873 ) ;
#1875 = CARTESIAN_POINT ( 'NONE',  ( -72.12500000204839523, 44.30836144126050158, -25.81189881249999374 ) ) ;
#1876 = CARTESIAN_POINT ( 'NONE',  ( -17.00387655282055377, 69.86881140706658755, 14.86941770366936311 ) ) ;
#1877 = MECHANICAL_DESIGN_GEOMETRIC_PRESENTATION_REPRESENTATION (  '', ( #6123 ), #11251 ) ;
#1878 = CARTESIAN_POINT ( 'NONE',  ( -80.00000000000002842, 42.27207793864211283, 4.242644059037075976 ) ) ;
#1879 = VERTEX_POINT ( 'NONE', #99 ) ;
#1880 = CARTESIAN_POINT ( 'NONE',  ( -7.706467115899972242, 56.60995633697762486, -4.745024238781081927 ) ) ;
#1881 = EDGE_CURVE ( 'NONE', #494, #7502, #39, .T. ) ;
#1882 = CARTESIAN_POINT ( 'NONE',  ( 0.8268573817076104726, 37.44832105976551873, -11.71822709476406210 ) ) ;
#1883 = ORIENTED_EDGE ( 'NONE', *, *, #3862, .F. ) ;
#1884 = CARTESIAN_POINT ( 'NONE',  ( -29.33720989395294509, 35.57257717978642830, 8.046635596291469739 ) ) ;
#1885 = CIRCLE ( 'NONE', #3057, 1.500000000000001332 ) ;
#1886 = CARTESIAN_POINT ( 'NONE',  ( -25.18906244525692983, 49.50751464484449826, 20.43480895838654376 ) ) ;
#1887 = CARTESIAN_POINT ( 'NONE',  ( -5.000000000000000000, -2.417244626924487605, -0.3110470720778656939 ) ) ;
#1888 = CARTESIAN_POINT ( 'NONE',  ( -79.43750000204838102, 55.00000000000000000, -25.81189881249999729 ) ) ;
#1889 = CIRCLE ( 'NONE', #6318, 21.50000000000000000 ) ;
#1890 = DIRECTION ( 'NONE',  ( 0.000000000000000000, 0.000000000000000000, 1.000000000000000000 ) ) ;
#1891 = DIRECTION ( 'NONE',  ( -1.000000000000000000, 0.000000000000000000, 0.000000000000000000 ) ) ;
#1892 = ORIENTED_EDGE ( 'NONE', *, *, #4690, .T. ) ;
#1893 = CARTESIAN_POINT ( 'NONE',  ( -71.37500000409677625, 55.00000000000000000, -24.99999999999999645 ) ) ;
#1894 = CARTESIAN_POINT ( 'NONE',  ( -20.57640403573022780, 55.00362648708293989, 0.004766381080466141652 ) ) ;
#1895 = PRODUCT_DEFINITION ( 'UNKNOWN', '', #7575, #7866 ) ;
#1896 = CARTESIAN_POINT ( 'NONE',  ( -54.93158096975896143, 57.64487218557030701, 4.246342238008629977 ) ) ;
#1897 = CIRCLE ( 'NONE', #11650, 2.500000000000000000 ) ;
#1898 = CYLINDRICAL_SURFACE ( 'NONE', #11310, 4.999999999999984013 ) ;
#1899 = CARTESIAN_POINT ( 'NONE',  ( -78.12500000409677625, 55.00000000000000000, 24.99999999999999645 ) ) ;
#1900 = EDGE_LOOP ( 'NONE', ( #3688, #6429 ) ) ;
#1901 = CARTESIAN_POINT ( 'NONE',  ( -7.070747353360942178, 68.33360022464046324, -16.24461469319379603 ) ) ;
#1902 = CARTESIAN_POINT ( 'NONE',  ( -72.78125000204838102, 55.00000000000000000, 25.81189881249999729 ) ) ;
#1903 = EDGE_CURVE ( 'NONE', #1507, #3923, #11671, .T. ) ;
#1904 = CARTESIAN_POINT ( 'NONE',  ( -29.87222872871134527, 51.02501382459326607, 3.050615963077655035 ) ) ;
#1905 = PLANE ( 'NONE',  #9512 ) ;
#1906 = CARTESIAN_POINT ( 'NONE',  ( -23.32960838815753490, 78.33373921288500696, -8.983038135490025056 ) ) ;
#1907 = DIRECTION ( 'NONE',  ( -1.000000000000000000, 0.000000000000000000, 0.000000000000000000 ) ) ;
#1908 = AXIS2_PLACEMENT_3D ( 'NONE', #4429, #10814, #3638 ) ;
#1909 = ORIENTED_EDGE ( 'NONE', *, *, #869, .F. ) ;
#1910 = CARTESIAN_POINT ( 'NONE',  ( -78.40625000204839523, 36.74823131438026280, 18.25176868561974786 ) ) ;
#1911 = VERTEX_POINT ( 'NONE', #2699 ) ;
#1912 = CARTESIAN_POINT ( 'NONE',  ( -6.515206263428001243, 58.30176811177454255, -3.769010736591787314 ) ) ;
#1913 = CARTESIAN_POINT ( 'NONE',  ( -18.99814003679748708, 60.36334191107018654, 12.94714326548398731 ) ) ;
#1914 = ADVANCED_FACE ( 'NONE', ( #7318 ), #10945, .F. ) ;
#1915 = EDGE_CURVE ( 'NONE', #2443, #3965, #6530, .T. ) ;
#1916 = CARTESIAN_POINT ( 'NONE',  ( 36.99999999999999289, 55.00000000000000000, 0.000000000000000000 ) ) ;
#1917 = CARTESIAN_POINT ( 'NONE',  ( -75.00000000000001421, 72.60765915417964322, -18.52300487688723152 ) ) ;
#1918 = CIRCLE ( 'NONE', #3844, 1.500000000000001332 ) ;
#1919 = FACE_OUTER_BOUND ( 'NONE', #5973, .T. ) ;
#1920 = ORIENTED_EDGE ( 'NONE', *, *, #5579, .T. ) ;
#1921 = AXIS2_PLACEMENT_3D ( 'NONE', #8467, #1141, #6679 ) ;
#1922 = CARTESIAN_POINT ( 'NONE',  ( -74.28125000000007105, 30.00000000000014211, -10.35533905932732601 ) ) ;
#1923 = CARTESIAN_POINT ( 'NONE',  ( -77.84375000409677625, 30.00000000000001421, 10.35533905932739174 ) ) ;
#1924 = CARTESIAN_POINT ( 'NONE',  ( 6.123233995736761352E-16, -17.82799999999998875, 4.999999999999995559 ) ) ;
#1925 = AXIS2_PLACEMENT_3D ( 'NONE', #406, #4973, #9270 ) ;
#1926 = CARTESIAN_POINT ( 'NONE',  ( -35.42605725946955886, 54.98265126924874124, -0.01969512534468634626 ) ) ;
#1927 = APPLICATION_PROTOCOL_DEFINITION ( 'draft international standard', 'automotive_design', 1998, #2255 ) ;
#1928 = CARTESIAN_POINT ( 'NONE',  ( -5.007765583651338837, 65.88190602726542977, -19.12178772468223897 ) ) ;
#1929 = CIRCLE ( 'NONE', #8641, 2.500000000000000000 ) ;
#1930 = DIRECTION ( 'NONE',  ( -1.000000000000000000, -0.000000000000000000, -0.000000000000000000 ) ) ;
#1931 = EDGE_LOOP ( 'NONE', ( #5144, #6420, #8047, #4868 ) ) ;
#1932 = CARTESIAN_POINT ( 'NONE',  ( -79.62500000000001421, 79.99999999999997158, -1.530808498934189944E-15 ) ) ;
#1933 = CARTESIAN_POINT ( 'NONE',  ( -73.90625000409680467, 80.00000000000001421, 10.35533905932737397 ) ) ;
#1934 = ORIENTED_EDGE ( 'NONE', *, *, #4687, .F. ) ;
#1935 = CARTESIAN_POINT ( 'NONE',  ( -9.070746587277097817, 68.33487957594263662, -16.24597445391072270 ) ) ;
#1936 = CARTESIAN_POINT ( 'NONE',  ( -78.31250000204839523, 29.18810118750000981, 10.69163855873950020 ) ) ;
#1937 = VECTOR ( 'NONE', #3474, 1000.000000000000000 ) ;
#1938 = VECTOR ( 'NONE', #11031, 1000.000000000000000 ) ;
#1939 = EDGE_LOOP ( 'NONE', ( #5728, #5478, #8347, #5802 ) ) ;
#1940 = FACE_OUTER_BOUND ( 'NONE', #4242, .T. ) ;
#1941 = CARTESIAN_POINT ( 'NONE',  ( -22.47759590436300314, 52.25445647903773505, 21.02373912143526979 ) ) ;
#1942 = CLOSED_SHELL ( 'NONE', ( #6086, #7241, #2159, #1410, #1619, #9768, #5316, #10444, #2047, #4900, #1547, #8436, #6698, #948, #7896, #1337, #6978, #427, #5335, #5578, #73, #2882, #9885, #3822, #4820, #11851, #437, #1225, #5185, #3966, #9168, #2788, #11339, #4188, #5295, #7143, #5894, #1146, #7469, #2200, #9443, #10633, #7710, #4333, #10036, #6330 ) ) ;
#1943 = CARTESIAN_POINT ( 'NONE',  ( -36.47762819585614835, 42.07544065584382764, -16.80749884933775462 ) ) ;
#1944 = ORIENTED_EDGE ( 'NONE', *, *, #6664, .T. ) ;
#1945 = CARTESIAN_POINT ( 'NONE',  ( 2.500000000000000000, 0.000000000000000000, -6.099999999999999645 ) ) ;
#1946 = CARTESIAN_POINT ( 'NONE',  ( -72.68750000409677625, 72.67766952966368876, -17.67766952966368876 ) ) ;
#1947 = CARTESIAN_POINT ( 'NONE',  ( 63.00000000000000000, 55.00000000000000000, 0.000000000000000000 ) ) ;
#1948 = VERTEX_POINT ( 'NONE', #6364 ) ;
#1949 = CARTESIAN_POINT ( 'NONE',  ( -19.11869220366278199, 65.80735234221702967, 18.02962863481653955 ) ) ;
#1950 = CARTESIAN_POINT ( 'NONE',  ( -57.50627882723209439, 66.73110044028416610, 17.54296274220338958 ) ) ;
#1951 = CARTESIAN_POINT ( 'NONE',  ( -72.87500000409677625, 55.00000000000000000, -24.99999999999999645 ) ) ;
#1952 = DIRECTION ( 'NONE',  ( 0.000000000000000000, 0.000000000000000000, -1.000000000000000000 ) ) ;
#1953 = DIRECTION ( 'NONE',  ( 1.000000000000000000, 6.033820786006286457E-17, -0.000000000000000000 ) ) ;
#1954 = DIRECTION ( 'NONE',  ( -1.000000000000000000, -0.000000000000000000, -0.000000000000000000 ) ) ;
#1955 = VERTEX_POINT ( 'NONE', #7498 ) ;
#1956 = DIRECTION ( 'NONE',  ( 0.000000000000000000, 1.000000000000000000, 0.000000000000000000 ) ) ;
#1957 = CARTESIAN_POINT ( 'NONE',  ( -32.53821616509017645, 54.99747915939720144, 0.0007716475280872252956 ) ) ;
#1958 = CARTESIAN_POINT ( 'NONE',  ( -51.62174940093352404, 59.49509050522294729, 2.214026401944775735 ) ) ;
#1959 = EDGE_CURVE ( 'NONE', #9573, #11173, #10525, .T. ) ;
#1960 = LINE ( 'NONE', #9388, #7831 ) ;
#1961 = CARTESIAN_POINT ( 'NONE',  ( -78.31250000409679046, 72.67766952966368876, 17.67766952966368521 ) ) ;
#1962 = CARTESIAN_POINT ( 'NONE',  ( -60.16384031450671444, 57.73999876476588611, 13.79403801089012660 ) ) ;
#1963 = ORIENTED_EDGE ( 'NONE', *, *, #3528, .T. ) ;
#1964 = DIRECTION ( 'NONE',  ( -1.000000000000000000, -0.000000000000000000, -0.000000000000000000 ) ) ;
#1965 = DIRECTION ( 'NONE',  ( 0.000000000000000000, 0.000000000000000000, 1.000000000000000000 ) ) ;
#1966 = CARTESIAN_POINT ( 'NONE',  ( -32.21076886968869246, 50.12793110694000376, 1.301955266658537003 ) ) ;
#1967 = CARTESIAN_POINT ( 'NONE',  ( 53.00000000000000000, 105.0000000000000142, 0.000000000000000000 ) ) ;
#1968 = CARTESIAN_POINT ( 'NONE',  ( -73.81250000204839523, 29.18810118750000626, -10.69163855873949309 ) ) ;
#1969 = CARTESIAN_POINT ( 'NONE',  ( -77.65625000204839523, 73.25176868561975141, -18.25176868561974430 ) ) ;
#1970 = VERTEX_POINT ( 'NONE', #7370 ) ;
#1971 = FACE_OUTER_BOUND ( 'NONE', #1220, .T. ) ;
#1972 = ORIENTED_EDGE ( 'NONE', *, *, #6412, .T. ) ;
#1973 = CARTESIAN_POINT ( 'NONE',  ( -15.00000000000000355, 5.000000000000000000, 30.00000000000000711 ) ) ;
#1974 = CARTESIAN_POINT ( 'NONE',  ( -59.25590502003253590, 53.62714168963238848, 13.95829701047152405 ) ) ;
#1975 = PLANE ( 'NONE',  #3660 ) ;
#1976 = CARTESIAN_POINT ( 'NONE',  ( 0.000000000000000000, 0.000000000000000000, -6.099999999999999645 ) ) ;
#1977 = CARTESIAN_POINT ( 'NONE',  ( -78.00000000000001421, 54.99999999999999289, -16.97055937655931501 ) ) ;
#1978 = ORIENTED_EDGE ( 'NONE', *, *, #7125, .F. ) ;
#1979 = CARTESIAN_POINT ( 'NONE',  ( -80.00000000000000000, 55.00000000000000000, -24.99999999999999645 ) ) ;
#1980 = CARTESIAN_POINT ( 'NONE',  ( -76.90625000409677625, 80.00000000000001421, 10.35533905932737397 ) ) ;
#1981 = ADVANCED_FACE ( 'NONE', ( #9100 ), #7435, .T. ) ;
#1982 = CARTESIAN_POINT ( 'NONE',  ( -33.95704062082862862, 50.00000000000001421, -0.1649495599488684516 ) ) ;
#1983 = CONICAL_SURFACE ( 'NONE', #5441, 3.000000000000000000, 0.9599310885968912466 ) ;
#1984 = FACE_BOUND ( 'NONE', #10175, .T. ) ;
#1985 = CARTESIAN_POINT ( 'NONE',  ( -7.291280311133348846, 60.19918483626972971, -4.712039246562317096 ) ) ;
#1986 = ITEM_DEFINED_TRANSFORMATION ( 'NONE', 'NONE', #6997,  #4738 ) ;
#1987 = FACE_OUTER_BOUND ( 'NONE', #8654, .T. ) ;
#1988 = FACE_OUTER_BOUND ( 'NONE', #5112, .T. ) ;
#1989 = ADVANCED_FACE ( 'NONE', ( #8205 ), #4601, .T. ) ;
#1990 = ORIENTED_EDGE ( 'NONE', *, *, #7700, .F. ) ;
#1991 = CARTESIAN_POINT ( 'NONE',  ( -79.53125000000001421, 79.99999999999998579, 10.35533905932735799 ) ) ;
#1992 = CARTESIAN_POINT ( 'NONE',  ( 36.99999999999999289, 55.00000000000000000, 0.000000000000000000 ) ) ;
#1993 = EDGE_LOOP ( 'NONE', ( #1978, #9827, #1296, #10861 ) ) ;
#1994 = CARTESIAN_POINT ( 'NONE',  ( -5.608280846031337141, 57.05942937149918492, -21.01412426850803783 ) ) ;
#1995 = CARTESIAN_POINT ( 'NONE',  ( -73.43750000204839523, 65.69163855873948421, -25.81189881250000440 ) ) ;
#1996 = CARTESIAN_POINT ( 'NONE',  ( 39.99999999999999289, 55.00000000000000000, 24.99999999999999645 ) ) ;
#1997 = CARTESIAN_POINT ( 'NONE',  ( -15.27494751580540111, 73.62981360231496808, 9.945832149094092856 ) ) ;
#1998 =( LENGTH_UNIT ( ) NAMED_UNIT ( * ) SI_UNIT ( .MILLI., .METRE. ) );
#1999 = CARTESIAN_POINT ( 'NONE',  ( -59.00490307935969270, 55.00061426705308065, 21.02882928537637497 ) ) ;
#2000 = EDGE_LOOP ( 'NONE', ( #11386, #9598, #3097, #7550 ) ) ;
#2001 = DIRECTION ( 'NONE',  ( 0.000000000000000000, 0.000000000000000000, 1.000000000000000000 ) ) ;
#2002 = CARTESIAN_POINT ( 'NONE',  ( -6.152294610831279265, 55.33101663292276129, -5.000007508712183579 ) ) ;
#2003 = CARTESIAN_POINT ( 'NONE',  ( -7.337209909475700620, 63.04728967918421745, -19.42673836724018699 ) ) ;
#2004 = VERTEX_POINT ( 'NONE', #1006 ) ;
#2005 = CARTESIAN_POINT ( 'NONE',  ( -43.32947769439600449, 63.04458385766601936, -19.42270034872903750 ) ) ;
#2006 = CARTESIAN_POINT ( 'NONE',  ( 14.12709322831273795, 56.83099522254385505, 13.98200332532292123 ) ) ;
#2007 = DIRECTION ( 'NONE',  ( -0.000000000000000000, -1.000000000000000000, -0.000000000000000000 ) ) ;
#2008 = CARTESIAN_POINT ( 'NONE',  ( -77.65625000409676204, 30.00000000000000355, -10.35533905932738108 ) ) ;
#2009 = CYLINDRICAL_SURFACE ( 'NONE', #1711, 22.00000000000000000 ) ;
#2010 = DIRECTION ( 'NONE',  ( 0.8191520442889885789, 0.000000000000000000, 0.5735764363510507113 ) ) ;
#2011 = ORIENTED_EDGE ( 'NONE', *, *, #10767, .T. ) ;
#2012 = CARTESIAN_POINT ( 'NONE',  ( -76.06250000000000000, 37.32233047033631124, 17.67766952966369232 ) ) ;
#2013 = CARTESIAN_POINT ( 'NONE',  ( -45.66879787574058724, 54.99910181478063009, 0.001600114446596862059 ) ) ;
#2014 = CARTESIAN_POINT ( 'NONE',  ( -48.51431238046460237, 59.99999999999936051, -0.3319244779807851708 ) ) ;
#2015 = SURFACE_SIDE_STYLE ('',( #2078 ) ) ;
#2016 = VECTOR ( 'NONE', #1478, 1000.000000000000000 ) ;
#2017 = DIRECTION ( 'NONE',  ( 0.000000000000000000, 1.000000000000000000, 0.000000000000000000 ) ) ;
#2018 = CARTESIAN_POINT ( 'NONE',  ( -4.109914231205427981, 53.16120966094572964, -6.833699982310251109 ) ) ;
#2019 = EDGE_LOOP ( 'NONE', ( #5337, #2089, #3376, #6161 ) ) ;
#2020 = CARTESIAN_POINT ( 'NONE',  ( 2.274842917244503937, 38.70728229458904934, -13.38060881307704975 ) ) ;
#2021 = CARTESIAN_POINT ( 'NONE',  ( 47.00000000000000000, 51.46446609406726935, 3.535533905932731091 ) ) ;
#2022 = CARTESIAN_POINT ( 'NONE',  ( -30.65099889004999412, 50.66178966001721307, 2.507330033107963985 ) ) ;
#2023 = DIRECTION ( 'NONE',  ( -1.000000000000000000, -0.000000000000000000, -0.000000000000000000 ) ) ;
#2024 = EDGE_CURVE ( 'NONE', #364, #8530, #1351, .T. ) ;
#2025 = CARTESIAN_POINT ( 'NONE',  ( -17.84886775434581452, 73.89817018583475772, -16.37880432067737146 ) ) ;
#2026 = CARTESIAN_POINT ( 'NONE',  ( -72.03125000204838102, 55.00000000000000000, -25.81189881249999729 ) ) ;
#2027 = ORIENTED_EDGE ( 'NONE', *, *, #9346, .T. ) ;
#2028 = CARTESIAN_POINT ( 'NONE',  ( -73.43750000204839523, 44.30836144126050158, -25.81189881249999374 ) ) ;
#2029 = EDGE_LOOP ( 'NONE', ( #3742, #691, #10930, #8070 ) ) ;
#2030 = CARTESIAN_POINT ( 'NONE',  ( 14.93568603768559200, 71.73165937744515475, -18.58548037958608390 ) ) ;
#2031 = CARTESIAN_POINT ( 'NONE',  ( -29.21146697695694527, 41.39918523644610104, 3.407148991788945924 ) ) ;
#2032 = AXIS2_PLACEMENT_3D ( 'NONE', #11264, #3076, #6746 ) ;
#2033 = EDGE_CURVE ( 'NONE', #10958, #2110, #4494, .T. ) ;
#2034 = CARTESIAN_POINT ( 'NONE',  ( 0.000000000000000000, 0.000000000000000000, -6.099999999999999645 ) ) ;
#2035 = DIRECTION ( 'NONE',  ( -1.000000000000000000, -0.000000000000000000, -0.000000000000000000 ) ) ;
#2036 = CARTESIAN_POINT ( 'NONE',  ( -15.00000000000000355, 0.000000000000000000, 30.00000000000000711 ) ) ;
#2037 = ORIENTED_EDGE ( 'NONE', *, *, #899, .F. ) ;
#2038 = PRODUCT ( 'perforated grinding plate', 'perforated grinding plate', '', ( #6496 ) ) ;
#2039 = VECTOR ( 'NONE', #4198, 1000.000000000000000 ) ;
#2040 = CARTESIAN_POINT ( 'NONE',  ( -78.68750000000001421, 37.32233047033631124, -17.67766952966368166 ) ) ;
#2041 = CARTESIAN_POINT ( 'NONE',  ( -71.46875000409677625, 44.64466094067260826, -24.99999999999998934 ) ) ;
#2042 = CIRCLE ( 'NONE', #4539, 1.500000000000001332 ) ;
#2043 = CARTESIAN_POINT ( 'NONE',  ( -34.54441260842353500, 50.04071390848193346, -0.6575957411896632410 ) ) ;
#2044 = FACE_BOUND ( 'NONE', #8189, .T. ) ;
#2045 = CARTESIAN_POINT ( 'NONE',  ( 7.000139726508040283, 47.98854375967137287, -0.0002567025502792563349 ) ) ;
#2046 = CARTESIAN_POINT ( 'NONE',  ( -16.77618538223333289, 72.99562347272558327, 12.71320776128724539 ) ) ;
#2047 = ADVANCED_FACE ( 'NONE', ( #11062 ), #4730, .T. ) ;
#2048 = CIRCLE ( 'NONE', #328, 3.000000000000000000 ) ;
#2049 = LINE ( 'NONE', #3728, #1645 ) ;
#2050 =( GEOMETRIC_REPRESENTATION_CONTEXT ( 3 ) GLOBAL_UNCERTAINTY_ASSIGNED_CONTEXT ( ( #2479 ) ) GLOBAL_UNIT_ASSIGNED_CONTEXT ( ( #11367, #1646, #5315 ) ) REPRESENTATION_CONTEXT ( 'NONE', 'WORKASPACE' ) );
#2051 = ORIENTED_EDGE ( 'NONE', *, *, #7567, .T. ) ;
#2052 = CARTESIAN_POINT ( 'NONE',  ( -5.000000000000000888, -1.936377641173858688, -5.902630826755077109 ) ) ;
#2053 = CARTESIAN_POINT ( 'NONE',  ( -74.28125000409677625, 65.35533905932754806, -24.99999999999982947 ) ) ;
#2054 = VERTEX_POINT ( 'NONE', #942 ) ;
#2055 = CARTESIAN_POINT ( 'NONE',  ( -20.73741325422386339, 64.90628579765783002, 18.53688757488948369 ) ) ;
#2056 = CARTESIAN_POINT ( 'NONE',  ( -78.00000000000002842, 46.51471862576140381, 6.985284746156355418 ) ) ;
#2057 = EDGE_CURVE ( 'NONE', #7726, #3451, #163, .T. ) ;
#2058 = EDGE_CURVE ( 'NONE', #1342, #678, #10330, .T. ) ;
#2059 = AXIS2_PLACEMENT_3D ( 'NONE', #9874, #2754, #10709 ) ;
#2060 = EDGE_CURVE ( 'NONE', #5404, #8475, #1479, .T. ) ;
#2061 = CARTESIAN_POINT ( 'NONE',  ( 53.00000000000000000, 105.0000000000000142, 6.000000000000000000 ) ) ;
#2062 = CARTESIAN_POINT ( 'NONE',  ( -51.69727455458300369, 74.78870212167194609, 7.080596778485133136 ) ) ;
#2063 = DIRECTION ( 'NONE',  ( 1.000000000000000000, 0.000000000000000000, 0.000000000000000000 ) ) ;
#2064 = ORIENTED_EDGE ( 'NONE', *, *, #10321, .F. ) ;
#2065 = CARTESIAN_POINT ( 'NONE',  ( -72.59375000204838102, 55.00000000000000000, 25.81189881249999729 ) ) ;
#2066 = CARTESIAN_POINT ( 'NONE',  ( -72.87500000409677625, 55.00000000000000000, -24.99999999999999645 ) ) ;
#2067 = CARTESIAN_POINT ( 'NONE',  ( -75.00000000000000000, 55.00000000000000000, 0.000000000000000000 ) ) ;
#2068 = ORIENTED_EDGE ( 'NONE', *, *, #7447, .F. ) ;
#2069 = CARTESIAN_POINT ( 'NONE',  ( -31.96936060593014162, 33.99278688086445044, -1.031647977713077813 ) ) ;
#2070 = CARTESIAN_POINT ( 'NONE',  ( -67.17448730496187181, 36.66801277209461318, 10.55271442276269944 ) ) ;
#2071 = CARTESIAN_POINT ( 'NONE',  ( -78.03125000409679046, 44.64466094067260826, 24.99999999999998579 ) ) ;
#2072 = CARTESIAN_POINT ( 'NONE',  ( -78.00000000000002842, 59.24264068711927678, 14.22792543327563131 ) ) ;
#2073 = DIRECTION ( 'NONE',  ( 1.000000000000000000, 0.000000000000000000, 0.000000000000000000 ) ) ;
#2074 = ORIENTED_EDGE ( 'NONE', *, *, #4284, .T. ) ;
#2075 = CARTESIAN_POINT ( 'NONE',  ( -75.12500000000000000, 80.00000000000000000, -1.530808498934191324E-15 ) ) ;
#2076 = CARTESIAN_POINT ( 'NONE',  ( -65.49460043985243374, 54.99687722424931025, 0.003115495885130020737 ) ) ;
#2077 = DIRECTION ( 'NONE',  ( 1.000000000000000000, 6.033820786006286457E-17, 0.000000000000000000 ) ) ;
#2078 = SURFACE_STYLE_FILL_AREA ( #4002 ) ;
#2079 = DIRECTION ( 'NONE',  ( 1.000000000000000000, 6.033820786006286457E-17, 0.000000000000000000 ) ) ;
#2080 = CARTESIAN_POINT ( 'NONE',  ( 18.44333507102063763, 60.58560716114385514, 4.289589058474648553 ) ) ;
#2081 = VECTOR ( 'NONE', #10977, 1000.000000000000000 ) ;
#2082 = ORIENTED_EDGE ( 'NONE', *, *, #3680, .F. ) ;
#2083 = CARTESIAN_POINT ( 'NONE',  ( 5.737308841168996310, 34.06700459503902323, -2.059191599423306318 ) ) ;
#2084 = LINE ( 'NONE', #9744, #9868 ) ;
#2085 = CARTESIAN_POINT ( 'NONE',  ( -80.00000000000001421, 63.48528137423857487, -6.985278002320760571 ) ) ;
#2086 = DIRECTION ( 'NONE',  ( 0.000000000000000000, 1.000000000000000000, 0.000000000000000000 ) ) ;
#2087 = CARTESIAN_POINT ( 'NONE',  ( 0.000000000000000000, -17.82799999999998875, 0.000000000000000000 ) ) ;
#2088 = CARTESIAN_POINT ( 'NONE',  ( -78.21875000204839523, 29.18810118750000271, 4.741568889096522788E-15 ) ) ;
#2089 = ORIENTED_EDGE ( 'NONE', *, *, #6623, .T. ) ;
#2090 = CARTESIAN_POINT ( 'NONE',  ( -73.34375000204839523, 55.00000000000000000, -25.81189881249999729 ) ) ;
#2091 = CONICAL_SURFACE ( 'NONE', #8793, 20.00000000000000000, 0.1745329251994333364 ) ;
#2092 = CARTESIAN_POINT ( 'NONE',  ( 14.99999999999999645, 0.000000000000000000, -29.99999999999999289 ) ) ;
#2093 = CARTESIAN_POINT ( 'NONE',  ( 1.711474602913919396, 65.50696799861361797, -22.68545269630726224 ) ) ;
#2094 = AXIS2_PLACEMENT_3D ( 'NONE', #3231, #8918, #2569 ) ;
#2095 = CARTESIAN_POINT ( 'NONE',  ( -56.92857623826265012, 59.09574567893412222, 13.47676509801295452 ) ) ;
#2096 = CARTESIAN_POINT ( 'NONE',  ( -79.43750000204838102, 65.69163855873948421, -25.81189881250000084 ) ) ;
#2097 = ADVANCED_FACE ( 'NONE', ( #9255 ), #4648, .F. ) ;
#2098 = APPLICATION_CONTEXT ( 'automotive_design' ) ;
#2099 = DIRECTION ( 'NONE',  ( -1.000000000000000000, -0.000000000000000000, -0.000000000000000000 ) ) ;
#2100 = DIRECTION ( 'NONE',  ( -1.000000000000000000, -0.000000000000000000, -0.000000000000000000 ) ) ;
#2101 = AXIS2_PLACEMENT_3D ( 'NONE', #9621, #10568, #7716 ) ;
#2102 = EDGE_LOOP ( 'NONE', ( #11444, #8277 ) ) ;
#2103 = DIRECTION ( 'NONE',  ( -1.000000000000000000, -0.000000000000000000, -0.000000000000000000 ) ) ;
#2104 = CARTESIAN_POINT ( 'NONE',  ( -72.78125000409679046, 65.35533905932737753, -24.99999999999999645 ) ) ;
#2105 = CARTESIAN_POINT ( 'NONE',  ( -41.15537497174283743, 53.39487353770535805, -4.746796348801736620 ) ) ;
#2106 = CARTESIAN_POINT ( 'NONE',  ( -3.500223734511656026, 56.37227171202499676, -6.892880562731030558 ) ) ;
#2107 = AXIS2_PLACEMENT_3D ( 'NONE', #1947, #11156, #10084 ) ;
#2108 = CARTESIAN_POINT ( 'NONE',  ( -72.78125000000008527, 30.00000000000014566, -10.35533905932732424 ) ) ;
#2109 = CARTESIAN_POINT ( 'NONE',  ( 39.99999999999999289, 55.00000000000000000, 0.000000000000000000 ) ) ;
#2110 = VERTEX_POINT ( 'NONE', #264 ) ;
#2111 = FACE_OUTER_BOUND ( 'NONE', #8407, .T. ) ;
#2112 = VECTOR ( 'NONE', #8051, 1000.000000000000000 ) ;
#2113 = DIRECTION ( 'NONE',  ( -1.000000000000000000, -0.000000000000000000, -0.000000000000000000 ) ) ;
#2114 = ORIENTED_EDGE ( 'NONE', *, *, #2937, .T. ) ;
#2115 = CARTESIAN_POINT ( 'NONE',  ( -28.94161417925737823, 38.68453375511723635, 13.40299329694203578 ) ) ;
#2116 = CIRCLE ( 'NONE', #3470, 2.981862520314375153 ) ;
#2117 = CARTESIAN_POINT ( 'NONE',  ( -75.31250000204839523, 29.18810118750000981, 10.69163855873950020 ) ) ;
#2118 = DIRECTION ( 'NONE',  ( -1.000000000000000000, 0.000000000000000000, 0.000000000000000000 ) ) ;
#2119 = CARTESIAN_POINT ( 'NONE',  ( -79.34375000000000000, 65.35533905932734910, 24.99999999999997158 ) ) ;
#2120 = CIRCLE ( 'NONE', #1358, 1.500000000000001332 ) ;
#2121 = VECTOR ( 'NONE', #4741, 1000.000000000000000 ) ;
#2122 = SURFACE_SIDE_STYLE ('',( #9552 ) ) ;
#2123 = CARTESIAN_POINT ( 'NONE',  ( -78.12500000409677625, 55.00000000000000000, 24.99999999999999645 ) ) ;
#2124 = ORIENTED_EDGE ( 'NONE', *, *, #6188, .T. ) ;
#2125 = CARTESIAN_POINT ( 'NONE',  ( -72.87500000204839523, 80.81189881250000440, 10.69163855873948243 ) ) ;
#2126 = EDGE_CURVE ( 'NONE', #10943, #5071, #8484, .T. ) ;
#2127 = CARTESIAN_POINT ( 'NONE',  ( 3.180458482999132919, 49.99999999999981526, -0.3308461596649949210 ) ) ;
#2128 = DIRECTION ( 'NONE',  ( 0.000000000000000000, 0.000000000000000000, 1.000000000000000000 ) ) ;
#2129 = ORIENTED_EDGE ( 'NONE', *, *, #10157, .F. ) ;
#2130 = CARTESIAN_POINT ( 'NONE',  ( 12.81090570363319436, 49.50804083114603316, 20.43325688243531602 ) ) ;
#2131 = AXIS2_PLACEMENT_3D ( 'NONE', #3234, #4132, #5275 ) ;
#2132 = CARTESIAN_POINT ( 'NONE',  ( -56.32961277634869646, 69.86611656190129338, 14.86520567151240080 ) ) ;
#2133 = AXIS2_PLACEMENT_3D ( 'NONE', #5955, #5108, #10649 ) ;
#2134 = CARTESIAN_POINT ( 'NONE',  ( -75.00000000000000000, 55.00000000000000000, 0.000000000000000000 ) ) ;
#2135 = CARTESIAN_POINT ( 'NONE',  ( 2.500000000000000000, 0.000000000000000000, -3.832189483390572970 ) ) ;
#2136 = DIRECTION ( 'NONE',  ( 0.000000000000000000, 0.000000000000000000, 1.000000000000000000 ) ) ;
#2137 = DIRECTION ( 'NONE',  ( -1.000000000000000000, 0.000000000000000000, 0.000000000000000000 ) ) ;
#2138 = EDGE_CURVE ( 'NONE', #4578, #911, #4217, .T. ) ;
#2139 = VERTEX_POINT ( 'NONE', #4891 ) ;
#2140 = CARTESIAN_POINT ( 'NONE',  ( -74.84375000000000000, 65.35533905932737753, 24.99999999999999645 ) ) ;
#2141 = DIRECTION ( 'NONE',  ( -0.8191520442889911324, 1.003171929053523884E-16, 0.5735764363510470476 ) ) ;
#2142 = CIRCLE ( 'NONE', #8635, 22.00000000000000000 ) ;
#2143 = CYLINDRICAL_SURFACE ( 'NONE', #4623, 1.500000000000000000 ) ;
#2144 = DIRECTION ( 'NONE',  ( -1.000000000000000000, 0.000000000000000000, 0.000000000000000000 ) ) ;
#2145 = CARTESIAN_POINT ( 'NONE',  ( -63.66377439455398246, 49.63604620300440473, 12.94636655892279009 ) ) ;
#2146 = ORIENTED_EDGE ( 'NONE', *, *, #1092, .T. ) ;
#2147 = CARTESIAN_POINT ( 'NONE',  ( -23.18906244097991021, 49.50939288222085821, 20.43027456479002879 ) ) ;
#2148 = CARTESIAN_POINT ( 'NONE',  ( -78.00000000000001421, 50.75735931288069480, -2.742637315201482462 ) ) ;
#2149 = CARTESIAN_POINT ( 'NONE',  ( -78.00000000000002842, 50.75735931288069480, 14.22792543327563131 ) ) ;
#2150 = CARTESIAN_POINT ( 'NONE',  ( 0.000000000000000000, 0.000000000000000000, -0.8895714285714284575 ) ) ;
#2151 = CARTESIAN_POINT ( 'NONE',  ( -14.31771318061109532, 71.29407831320283151, 18.96900533006995104 ) ) ;
#2152 = CARTESIAN_POINT ( 'NONE',  ( -74.00000000204839523, 29.18810118750000981, 10.69163855873950020 ) ) ;
#2153 = ORIENTED_EDGE ( 'NONE', *, *, #1324, .T. ) ;
#2154 = CARTESIAN_POINT ( 'NONE',  ( -72.12500000204840944, 29.18810118750000626, -10.69163855873949309 ) ) ;
#2155 = ORIENTED_EDGE ( 'NONE', *, *, #1692, .F. ) ;
#2156 = CARTESIAN_POINT ( 'NONE',  ( 25.27762860081886487, 79.98954112471153621, -0.8412697711426854186 ) ) ;
#2157 = CARTESIAN_POINT ( 'NONE',  ( -54.29700862423385388, 64.41868735558820447, 10.39170421311061254 ) ) ;
#2158 = CARTESIAN_POINT ( 'NONE',  ( -78.00000000000001421, 63.48528137423857487, 8.485284746156350977 ) ) ;
#2159 = ADVANCED_FACE ( 'NONE', ( #208 ), #6725, .F. ) ;
#2160 = DIRECTION ( 'NONE',  ( -1.000000000000000000, -0.000000000000000000, -0.000000000000000000 ) ) ;
#2161 = CARTESIAN_POINT ( 'NONE',  ( -78.00000000000002842, 59.24264068711927678, 11.22792543327563131 ) ) ;
#2162 = ORIENTED_EDGE ( 'NONE', *, *, #2057, .F. ) ;
#2163 = CARTESIAN_POINT ( 'NONE',  ( -75.96875000000000000, 30.00000000000001421, 10.35533905932739174 ) ) ;
#2164 = CARTESIAN_POINT ( 'NONE',  ( -73.71875000409677625, 65.35533905932737753, 24.99999999999999645 ) ) ;
#2165 = CARTESIAN_POINT ( 'NONE',  ( -38.81824253360387189, 51.69821110756454630, -3.768992944301960968 ) ) ;
#2166 = ORIENTED_EDGE ( 'NONE', *, *, #9821, .T. ) ;
#2167 = CARTESIAN_POINT ( 'NONE',  ( 24.10985792112495218, 61.79436671605726161, 1.822573681661085354 ) ) ;
#2168 = CARTESIAN_POINT ( 'NONE',  ( -17.79883679810149744, 73.80018128902068497, 11.43000178191448235 ) ) ;
#2169 = CARTESIAN_POINT ( 'NONE',  ( -78.00000000000002842, 42.27207793864211283, 12.72792543327562775 ) ) ;
#2170 = ORIENTED_EDGE ( 'NONE', *, *, #11241, .F. ) ;
#2171 = EDGE_CURVE ( 'NONE', #9767, #567, #3050, .T. ) ;
#2172 = DIRECTION ( 'NONE',  ( 1.000000000000000000, 0.000000000000000000, 0.000000000000000000 ) ) ;
#2173 = CARTESIAN_POINT ( 'NONE',  ( -76.81250000204838102, 29.18810118750000626, -10.69163855873949132 ) ) ;
#2174 = EDGE_LOOP ( 'NONE', ( #11721, #10327, #3071, #9481 ) ) ;
#2175 = CARTESIAN_POINT ( 'NONE',  ( -55.45210586135002728, 71.88485191958531573, 12.52183031059725771 ) ) ;
#2176 = SHAPE_REPRESENTATION ( 'Crank Handle', ( #4738 ), #4498 ) ;
#2177 = CARTESIAN_POINT ( 'NONE',  ( -74.09375000204839523, 55.00000000000000000, 25.81189881249999729 ) ) ;
#2178 = FACE_OUTER_BOUND ( 'NONE', #3367, .T. ) ;
#2179 = DIRECTION ( 'NONE',  ( 0.000000000000000000, 1.000000000000000000, 0.000000000000000000 ) ) ;
#2180 = FACE_OUTER_BOUND ( 'NONE', #9854, .T. ) ;
#2181 = ORIENTED_EDGE ( 'NONE', *, *, #4441, .F. ) ;
#2182 = CARTESIAN_POINT ( 'NONE',  ( -71.75000000204840944, 65.69163855873948421, -25.81189881250000084 ) ) ;
#2183 = EDGE_CURVE ( 'NONE', #6748, #6864, #10857, .T. ) ;
#2184 = DIRECTION ( 'NONE',  ( -1.000000000000000000, -0.000000000000000000, -0.000000000000000000 ) ) ;
#2185 = CARTESIAN_POINT ( 'NONE',  ( -25.18906244525692983, 49.50751464484449826, 20.43480895838654376 ) ) ;
#2186 = VERTEX_POINT ( 'NONE', #5477 ) ;
#2187 = CARTESIAN_POINT ( 'NONE',  ( -63.17697253202724283, 43.28183360602782415, 17.55497741318475491 ) ) ;
#2188 = CARTESIAN_POINT ( 'NONE',  ( 3.121866368482561160, 41.13189203504037295, -2.057008360219124032 ) ) ;
#2189 = LINE ( 'NONE', #5079, #10498 ) ;
#2190 = DIRECTION ( 'NONE',  ( 0.000000000000000000, 0.000000000000000000, 1.000000000000000000 ) ) ;
#2191 = LINE ( 'NONE', #9623, #7470 ) ;
#2192 = EDGE_CURVE ( 'NONE', #4978, #10867, #2886, .T. ) ;
#2193 = EDGE_LOOP ( 'NONE', ( #828, #7872 ) ) ;
#2194 = PLANE ( 'NONE',  #7492 ) ;
#2195 = DIRECTION ( 'NONE',  ( -1.000000000000000000, -0.000000000000000000, -0.000000000000000000 ) ) ;
#2196 =( BOUNDED_CURVE ( )  B_SPLINE_CURVE ( 2, ( #7999, #4161, #10613 ),
 .UNSPECIFIED., .F., .T. ) 
 B_SPLINE_CURVE_WITH_KNOTS ( ( 3, 3 ),
 ( 0.4166666666666670182, 0.4304371013617913633 ),
 .UNSPECIFIED. ) 
 CURVE ( )  GEOMETRIC_REPRESENTATION_ITEM ( )  RATIONAL_B_SPLINE_CURVE ( ( 0.9999999999999987788, 0.9496858275272472838, 0.9658850655769216642 ) ) 
 REPRESENTATION_ITEM ( '' )  );
#2197 = PRODUCT_DEFINITION ( 'UNKNOWN', '', #10978, #3306 ) ;
#2198 = ADVANCED_FACE ( 'NONE', ( #9905 ), #2546, .F. ) ;
#2199 =( GEOMETRIC_REPRESENTATION_CONTEXT ( 3 ) GLOBAL_UNCERTAINTY_ASSIGNED_CONTEXT ( ( #3996 ) ) GLOBAL_UNIT_ASSIGNED_CONTEXT ( ( #1998, #1764, #10023 ) ) REPRESENTATION_CONTEXT ( 'NONE', 'WORKASPACE' ) );
#2200 = ADVANCED_FACE ( 'NONE', ( #6212 ), #907, .T. ) ;
#2201 = EDGE_CURVE ( 'NONE', #6484, #4456, #1918, .T. ) ;
#2202 = DIRECTION ( 'NONE',  ( -1.000000000000000000, 0.000000000000000000, 0.000000000000000000 ) ) ;
#2203 = CARTESIAN_POINT ( 'NONE',  ( -70.67038125215350419, 40.99581249687635420, 0.003422455583789344152 ) ) ;
#2204 = ORIENTED_EDGE ( 'NONE', *, *, #3378, .F. ) ;
#2205 = CARTESIAN_POINT ( 'NONE',  ( -42.66281101964754896, 63.04450918361814615, -19.42252581123130639 ) ) ;
#2206 = CARTESIAN_POINT ( 'NONE',  ( 0.000000000000000000, 0.000000000000000000, -4.346257142857142597 ) ) ;
#2207 = DIRECTION ( 'NONE',  ( -1.000000000000000000, -0.000000000000000000, -0.000000000000000000 ) ) ;
#2208 = CARTESIAN_POINT ( 'NONE',  ( -78.12500000204839523, 29.18810118750000626, -10.69163855873949132 ) ) ;
#2209 = DIRECTION ( 'NONE',  ( 1.000000000000000000, 0.000000000000000000, 0.000000000000000000 ) ) ;
#2210 = CARTESIAN_POINT ( 'NONE',  ( -73.06250000204840944, 80.81189881250001861, 10.69163855873948599 ) ) ;
#2211 = EDGE_CURVE ( 'NONE', #3782, #1790, #1582, .T. ) ;
#2212 = EDGE_CURVE ( 'NONE', #10278, #11839, #4197, .T. ) ;
#2213 = VERTEX_POINT ( 'NONE', #3503 ) ;
#2214 = CARTESIAN_POINT ( 'NONE',  ( -72.96875000204838102, 80.81189881250000440, -1.580522963032174394E-15 ) ) ;
#2215 = CARTESIAN_POINT ( 'NONE',  ( 3.000000000000000888, 0.000000000000000000, -6.099999999999997868 ) ) ;
#2216 = EDGE_CURVE ( 'NONE', #2768, #9929, #10794, .T. ) ;
#2217 = CARTESIAN_POINT ( 'NONE',  ( -58.66904817996947941, 55.00018295349421749, 14.02051935868267307 ) ) ;
#2218 = CARTESIAN_POINT ( 'NONE',  ( -78.21875000204839523, 36.74823131438024859, -18.25176868561973720 ) ) ;
#2219 = FACE_OUTER_BOUND ( 'NONE', #1580, .T. ) ;
#2220 = CARTESIAN_POINT ( 'NONE',  ( -15.00000000000000000, 39.99999999999999289, -20.00000000000000000 ) ) ;
#2221 = ORIENTED_EDGE ( 'NONE', *, *, #8514, .F. ) ;
#2222 = AXIS2_PLACEMENT_3D ( 'NONE', #3167, #7958, #9803 ) ;
#2223 = CARTESIAN_POINT ( 'NONE',  ( -73.90625000000001421, 65.35533905932737753, -24.99999999999999645 ) ) ;
#2224 = CARTESIAN_POINT ( 'NONE',  ( -72.50000000409677625, 80.00000000000000000, -1.530808498934191324E-15 ) ) ;
#2225 = CIRCLE ( 'NONE', #4337, 4.171999999999999709 ) ;
#2226 = DIRECTION ( 'NONE',  ( -1.000000000000000000, 0.000000000000000000, 0.000000000000000000 ) ) ;
#2227 = ORIENTED_EDGE ( 'NONE', *, *, #9507, .F. ) ;
#2228 = CARTESIAN_POINT ( 'NONE',  ( 7.291299706434547723, 48.00851142473923971, 0.3439031866554066452 ) ) ;
#2229 = CARTESIAN_POINT ( 'NONE',  ( -80.00000000000002842, 46.51471862576140381, 3.371917798797308130E-06 ) ) ;
#2230 = CARTESIAN_POINT ( 'NONE',  ( 0.000000000000000000, 0.000000000000000000, -5.560532340533429263 ) ) ;
#2231 = ORIENTED_EDGE ( 'NONE', *, *, #4053, .T. ) ;
#2232 = CARTESIAN_POINT ( 'NONE',  ( -78.00000000000001421, 71.97056274847716395, 3.371917795327861178E-06 ) ) ;
#2233 = CARTESIAN_POINT ( 'NONE',  ( -76.06250000204839523, 80.81189881250000440, 10.69163855873948243 ) ) ;
#2234 = EDGE_LOOP ( 'NONE', ( #4086, #9591, #2051, #5911, #3105, #4250, #5327, #8599 ) ) ;
#2235 = CARTESIAN_POINT ( 'NONE',  ( -34.72515708538001888, 34.82355399787605421, -6.128525890628534256 ) ) ;
#2236 = CARTESIAN_POINT ( 'NONE',  ( 53.00000000000000000, 55.00000000000000000, 6.000000000000000000 ) ) ;
#2237 = DIRECTION ( 'NONE',  ( -0.000000000000000000, -0.000000000000000000, 1.000000000000000000 ) ) ;
#2238 = CARTESIAN_POINT ( 'NONE',  ( -67.52720549794999272, 34.02364409886038743, 2.748840581154547102 ) ) ;
#2239 = CONICAL_SURFACE ( 'NONE', #3974, 2.500000000000000000, 0.9599310885968755924 ) ;
#2240 = CARTESIAN_POINT ( 'NONE',  ( -80.00000000000001421, 59.24264068711927678, 2.742644059037073312 ) ) ;
#2241 = ORIENTED_EDGE ( 'NONE', *, *, #6430, .T. ) ;
#2242 = DIRECTION ( 'NONE',  ( 0.000000000000000000, 1.000000000000000000, 0.000000000000000000 ) ) ;
#2243 = CARTESIAN_POINT ( 'NONE',  ( -2.074714256722480776, 4.575665857285978966, -0.01055556052338894012 ) ) ;
#2244 = ADVANCED_FACE ( 'NONE', ( #2605 ), #2729, .F. ) ;
#2245 = CARTESIAN_POINT ( 'NONE',  ( -21.63602683877659771, 62.08561388645346568, 19.80191166437241179 ) ) ;
#2246 = ORIENTED_EDGE ( 'NONE', *, *, #797, .T. ) ;
#2247 = CARTESIAN_POINT ( 'NONE',  ( -15.18898619350627754, 75.43339460814846120, 5.491620057114340092 ) ) ;
#2248 = CARTESIAN_POINT ( 'NONE',  ( -1.460406270097956538, 46.38242329338708458, -11.20688125615216890 ) ) ;
#2249 = CYLINDRICAL_SURFACE ( 'NONE', #8030, 25.00000000000000355 ) ;
#2250 = LINE ( 'NONE', #330, #11759 ) ;
#2251 = LINE ( 'NONE', #10338, #8612 ) ;
#2252 = ORIENTED_EDGE ( 'NONE', *, *, #10689, .T. ) ;
#2253 = CARTESIAN_POINT ( 'NONE',  ( -79.71875000000001421, 80.00000000000001421, -10.35533905932737753 ) ) ;
#2254 = CARTESIAN_POINT ( 'NONE',  ( -60.23628175600274659, 55.00363048015435652, 0.01172028139553065243 ) ) ;
#2255 = APPLICATION_CONTEXT ( 'automotive_design' ) ;
#2256 = FACE_OUTER_BOUND ( 'NONE', #11356, .T. ) ;
#2257 = AXIS2_PLACEMENT_3D ( 'NONE', #1256, #2948, #3845 ) ;
#2258 = CARTESIAN_POINT ( 'NONE',  ( -75.00000000000000000, 55.00000000000000000, 0.000000000000000000 ) ) ;
#2259 = CARTESIAN_POINT ( 'NONE',  ( -41.83355676456199745, 53.63003671930656679, -6.894939712124843467 ) ) ;
#2260 = EDGE_LOOP ( 'NONE', ( #6399, #160, #887, #11432 ) ) ;
#2261 = CARTESIAN_POINT ( 'NONE',  ( -38.60828084422895046, 48.85949782923615459, -20.20603288453101243 ) ) ;
#2262 = DIRECTION ( 'NONE',  ( 0.000000000000000000, -1.000000000000000000, 0.000000000000000000 ) ) ;
#2263 = LINE ( 'NONE', #284, #458 ) ;
#2264 = CARTESIAN_POINT ( 'NONE',  ( -78.03125000204839523, 36.74823131438024859, -18.25176868561973720 ) ) ;
#2265 = DIRECTION ( 'NONE',  ( 0.000000000000000000, 0.000000000000000000, -1.000000000000000000 ) ) ;
#2266 = LINE ( 'NONE', #5940, #2293 ) ;
#2267 = ORIENTED_EDGE ( 'NONE', *, *, #7023, .T. ) ;
#2268 = CARTESIAN_POINT ( 'NONE',  ( -77.46875000409679046, 44.64466094067260826, -24.99999999999998934 ) ) ;
#2269 = CARTESIAN_POINT ( 'NONE',  ( -80.00000000000000000, 55.00000000000000000, -24.99999999999999645 ) ) ;
#2270 = CARTESIAN_POINT ( 'NONE',  ( -76.15625000000005684, 44.64466094067266511, 24.99999999999990408 ) ) ;
#2271 = SURFACE_STYLE_USAGE ( .BOTH. , #9026 ) ;
#2272 = CARTESIAN_POINT ( 'NONE',  ( 5.451907626115248817, 34.19820075889870026, -3.085388827037094828 ) ) ;
#2273 = CYLINDRICAL_SURFACE ( 'NONE', #1561, 1.500000000000000444 ) ;
#2274 = AXIS2_PLACEMENT_3D ( 'NONE', #1536, #9627, #6947 ) ;
#2275 = DIRECTION ( 'NONE',  ( 0.000000000000000000, 1.000000000000000000, 0.000000000000000000 ) ) ;
#2276 = EDGE_CURVE ( 'NONE', #2578, #6873, #3915, .T. ) ;
#2277 = CARTESIAN_POINT ( 'NONE',  ( -78.00000000000002842, 42.27207793864211283, 11.22792543327562775 ) ) ;
#2278 = ORIENTED_EDGE ( 'NONE', *, *, #4024, .T. ) ;
#2279 = CARTESIAN_POINT ( 'NONE',  ( -78.00000000000002842, 38.02943725152282184, -1.499996628082202133 ) ) ;
#2280 = PRODUCT_RELATED_PRODUCT_CATEGORY ( 'part', '', ( #1748 ) ) ;
#2281 = MECHANICAL_DESIGN_GEOMETRIC_PRESENTATION_REPRESENTATION (  '', ( #8140 ), #6886 ) ;
#2282 = CARTESIAN_POINT ( 'NONE',  ( -78.03124999999998579, 80.00000000000001421, 10.35533905932737397 ) ) ;
#2283 = DIRECTION ( 'NONE',  ( 1.000000000000000000, 6.033820786006286457E-17, -0.000000000000000000 ) ) ;
#2284 = AXIS2_PLACEMENT_3D ( 'NONE', #10192, #10528, #120 ) ;
#2285 = DIRECTION ( 'NONE',  ( -1.000000000000000000, 0.000000000000000000, 0.000000000000000000 ) ) ;
#2286 = EDGE_CURVE ( 'NONE', #5423, #10744, #2501, .T. ) ;
#2287 = ORIENTED_EDGE ( 'NONE', *, *, #913, .T. ) ;
#2288 = EDGE_CURVE ( 'NONE', #11145, #2349, #6247, .T. ) ;
#2289 = CARTESIAN_POINT ( 'NONE',  ( -58.33319328058090036, 54.99975163993536142, 7.012209431990541475 ) ) ;
#2290 = DIRECTION ( 'NONE',  ( 0.000000000000000000, 0.000000000000000000, 1.000000000000000000 ) ) ;
#2291 = CIRCLE ( 'NONE', #8992, 2.500000000000000000 ) ;
#2292 = DIRECTION ( 'NONE',  ( 1.000000000000000000, 0.000000000000000000, 0.000000000000000000 ) ) ;
#2293 = VECTOR ( 'NONE', #9580, 1000.000000000000000 ) ;
#2294 = ORIENTED_EDGE ( 'NONE', *, *, #5780, .T. ) ;
#2295 = CARTESIAN_POINT ( 'NONE',  ( 20.34144692743802807, 75.85564821147012537, -7.037142918007486259 ) ) ;
#2296 = CARTESIAN_POINT ( 'NONE',  ( -78.00000000000001421, 54.99999999999998579, -8.485278002320759683 ) ) ;
#2297 = ORIENTED_EDGE ( 'NONE', *, *, #291, .F. ) ;
#2298 = CARTESIAN_POINT ( 'NONE',  ( -72.21875000204838102, 29.18810118750000271, 4.741568889096522788E-15 ) ) ;
#2299 = CARTESIAN_POINT ( 'NONE',  ( -78.00000000000001421, 63.48528137423857487, -9.985278002320759683 ) ) ;
#2300 = CARTESIAN_POINT ( 'NONE',  ( -42.96936073659074395, 63.99245613053683712, -19.01383356661934343 ) ) ;
#2301 = CARTESIAN_POINT ( 'NONE',  ( -3.000000000000000000, 0.000000000000000000, -5.210428571428570521 ) ) ;
#2302 = ORIENTED_EDGE ( 'NONE', *, *, #2342, .T. ) ;
#2303 = DIRECTION ( 'NONE',  ( 0.000000000000000000, 0.000000000000000000, 1.000000000000000000 ) ) ;
#2304 = EDGE_CURVE ( 'NONE', #4836, #4164, #7465, .T. ) ;
#2305 = CIRCLE ( 'NONE', #7289, 1.500000000000001332 ) ;
#2306 = CARTESIAN_POINT ( 'NONE',  ( -30.36397657560652874, 35.99904827701746513, 8.986701095552454888 ) ) ;
#2307 = ORIENTED_EDGE ( 'NONE', *, *, #1685, .F. ) ;
#2308 = CARTESIAN_POINT ( 'NONE',  ( 3.262586490554605145, 34.88822117712475546, -6.102536506291977858 ) ) ;
#2309 = CARTESIAN_POINT ( 'NONE',  ( -44.41060717808029068, 59.06754546170965625, -13.40628650917997433 ) ) ;
#2310 = DIRECTION ( 'NONE',  ( 1.000000000000000000, 6.033820786006286457E-17, 0.000000000000000000 ) ) ;
#2311 = CARTESIAN_POINT ( 'NONE',  ( 39.99999999999999289, 55.00000000000000000, 0.000000000000000000 ) ) ;
#2312 = CIRCLE ( 'NONE', #9012, 2.500000000000000000 ) ;
#2313 = FACE_OUTER_BOUND ( 'NONE', #619, .T. ) ;
#2314 = CONICAL_SURFACE ( 'NONE', #969, 20.00000000000000000, 0.1745329251994333364 ) ;
#2315 = VERTEX_POINT ( 'NONE', #973 ) ;
#2316 = CARTESIAN_POINT ( 'NONE',  ( -71.99927368942448425, 76.65063862282433149, 12.49999388895319363 ) ) ;
#2317 = LINE ( 'NONE', #3107, #6259 ) ;
#2318 =( BOUNDED_CURVE ( )  B_SPLINE_CURVE ( 2, ( #2570, #7016, #10587, #2387, #9867, #1662, #586, #4253, #10639 ),
 .UNSPECIFIED., .F., .T. ) 
 B_SPLINE_CURVE_WITH_KNOTS ( ( 3, 2, 2, 2, 3 ),
 ( 0.7500000000000006661, 0.7708333333333340365, 0.7916666666666672958, 0.8125000000000006661, 0.8333333333333340365 ),
 .UNSPECIFIED. ) 
 CURVE ( )  GEOMETRIC_REPRESENTATION_ITEM ( )  RATIONAL_B_SPLINE_CURVE ( ( 0.9999999999999975575, 0.9238795325112891810, 1.000000000000000000, 0.9238795325112867385, 1.000000000000000000, 0.9238795325112867385, 1.000000000000000000, 0.9238795325112842960, 1.000000000000002442 ) ) 
 REPRESENTATION_ITEM ( '' )  );
#2319 = DIRECTION ( 'NONE',  ( 0.000000000000000000, 0.000000000000000000, 1.000000000000000000 ) ) ;
#2320 = AXIS2_PLACEMENT_3D ( 'NONE', #318, #8416, #10383 ) ;
#2321 = AXIS2_PLACEMENT_3D ( 'NONE', #2034, #3002, #9345 ) ;
#2322 = CARTESIAN_POINT ( 'NONE',  ( 3.000000000000000000, 3.673940397442059868E-16, -1.753742857142857048 ) ) ;
#2323 = CARTESIAN_POINT ( 'NONE',  ( -46.49982872022311398, 58.90684247826047937, -5.852054447348608690 ) ) ;
#2324 = EDGE_LOOP ( 'NONE', ( #8002, #10768, #10576, #6663 ) ) ;
#2325 = CARTESIAN_POINT ( 'NONE',  ( -21.05849041552747281, 57.05917194494736577, 20.98221040122819403 ) ) ;
#2326 = EDGE_CURVE ( 'NONE', #8979, #10562, #10255, .T. ) ;
#2327 = CLOSED_SHELL ( 'NONE', ( #8712, #5217, #8658, #10847, #4602, #10093, #4565, #4457, #1451, #1323, #9407, #808, #3976, #7463, #639, #2403, #8067, #3823, #11041, #3447, #3010, #7533, #266, #4848, #3457, #5436, #5812, #10805, #7204, #5209, #7295, #8665, #374 ) ) ;
#2328 = CARTESIAN_POINT ( 'NONE',  ( 19.85574934264614910, 73.36821619702706698, 10.58005382006121131 ) ) ;
#2329 = DIRECTION ( 'NONE',  ( -1.000000000000000000, -0.000000000000000000, -0.000000000000000000 ) ) ;
#2330 = CARTESIAN_POINT ( 'NONE',  ( -74.37500000204838102, 80.81189881250000440, 10.69163855873948243 ) ) ;
#2331 = CARTESIAN_POINT ( 'NONE',  ( -4.228830400747147777, 66.03037594905248397, 22.43534422001513207 ) ) ;
#2332 = CARTESIAN_POINT ( 'NONE',  ( -75.87500000204839523, 80.81189881250001861, 10.69163855873948599 ) ) ;
#2333 = ORIENTED_EDGE ( 'NONE', *, *, #3649, .F. ) ;
#2334 = EDGE_CURVE ( 'NONE', #1831, #8790, #6569, .T. ) ;
#2335 = CARTESIAN_POINT ( 'NONE',  ( -72.40625000409677625, 80.00000000000001421, 10.35533905932737397 ) ) ;
#2336 = DIRECTION ( 'NONE',  ( -0.000000000000000000, -0.000000000000000000, 1.000000000000000000 ) ) ;
#2337 = CONICAL_SURFACE ( 'NONE', #4060, 2.450000000000000178, 0.9599310885968801443 ) ;
#2338 = ORIENTED_EDGE ( 'NONE', *, *, #8504, .T. ) ;
#2339 = CARTESIAN_POINT ( 'NONE',  ( 10.18903847268274276, 38.19250115101311849, 12.92455934260550521 ) ) ;
#2340 = DIRECTION ( 'NONE',  ( 0.000000000000000000, 1.000000000000000000, 0.000000000000000000 ) ) ;
#2341 = DIRECTION ( 'NONE',  ( -1.000000000000000000, -0.000000000000000000, -0.000000000000000000 ) ) ;
#2342 = EDGE_CURVE ( 'NONE', #6241, #11230, #5789, .T. ) ;
#2343 = DIRECTION ( 'NONE',  ( -0.7071067811865519026, 8.659560562354878624E-17, -0.7071067811865431318 ) ) ;
#2344 = VERTEX_POINT ( 'NONE', #1869 ) ;
#2345 = DIRECTION ( 'NONE',  ( -0.000000000000000000, -1.000000000000000000, -0.000000000000000000 ) ) ;
#2346 = CARTESIAN_POINT ( 'NONE',  ( -75.12500000000000000, 80.00000000000000000, -1.530808498934191324E-15 ) ) ;
#2347 = FACE_OUTER_BOUND ( 'NONE', #7174, .T. ) ;
#2348 = FACE_OUTER_BOUND ( 'NONE', #11660, .T. ) ;
#2349 = VERTEX_POINT ( 'NONE', #2779 ) ;
#2350 = CARTESIAN_POINT ( 'NONE',  ( -26.24915659512696919, 49.55079243168071912, 4.477208298354541149 ) ) ;
#2351 = CARTESIAN_POINT ( 'NONE',  ( 0.000000000000000000, 0.000000000000000000, -2.968018054819144158 ) ) ;
#2352 = DIRECTION ( 'NONE',  ( 0.000000000000000000, 1.000000000000000000, 0.000000000000000000 ) ) ;
#2353 = EDGE_LOOP ( 'NONE', ( #10086, #5582, #6860, #5016 ) ) ;
#2354 = CARTESIAN_POINT ( 'NONE',  ( 21.71450277048158739, 76.99996143417730821, 0.3671359477368970614 ) ) ;
#2355 = CARTESIAN_POINT ( 'NONE',  ( -76.15625000204838102, 80.81189881250000440, -1.580522963032174394E-15 ) ) ;
#2356 = ORIENTED_EDGE ( 'NONE', *, *, #6842, .F. ) ;
#2357 = CARTESIAN_POINT ( 'NONE',  ( -73.34375000204839523, 55.00000000000000000, -25.81189881249999729 ) ) ;
#2358 = CARTESIAN_POINT ( 'NONE',  ( -75.40624999999991473, 65.35533905933888832, -24.99999999998830802 ) ) ;
#2359 = CARTESIAN_POINT ( 'NONE',  ( 0.000000000000000000, 0.000000000000000000, 0.000000000000000000 ) ) ;
#2360 = CARTESIAN_POINT ( 'NONE',  ( 3.236198281082953265, 55.01300725603349662, 0.01475152511819301064 ) ) ;
#2361 = CARTESIAN_POINT ( 'NONE',  ( -75.00000000000001421, 31.19324792593015871, 8.552347646381322832 ) ) ;
#2362 = EDGE_CURVE ( 'NONE', #4746, #1747, #6389, .T. ) ;
#2363 = VERTEX_POINT ( 'NONE', #8233 ) ;
#2364 = CARTESIAN_POINT ( 'NONE',  ( -78.00000000000001421, 54.99999999999999289, -16.97055937655931501 ) ) ;
#2365 = CARTESIAN_POINT ( 'NONE',  ( -20.45202553191040806, 65.80759480864719535, 18.03021102644938267 ) ) ;
#2366 = VERTEX_POINT ( 'NONE', #251 ) ;
#2367 = CARTESIAN_POINT ( 'NONE',  ( 22.14421007127711860, 75.43322280825043435, 5.492045153080157505 ) ) ;
#2368 = CARTESIAN_POINT ( 'NONE',  ( -11.73803863240502388, 67.39634740869848883, -6.621068033304872813 ) ) ;
#2369 = DIRECTION ( 'NONE',  ( -0.000000000000000000, -1.000000000000000000, -0.000000000000000000 ) ) ;
#2370 = CARTESIAN_POINT ( 'NONE',  ( -21.31755583740063287, 57.50727203353319794, 4.338243946322617894 ) ) ;
#2371 = EDGE_LOOP ( 'NONE', ( #10304, #5274 ) ) ;
#2372 = CARTESIAN_POINT ( 'NONE',  ( -78.21875000204839523, 36.74823131438024859, -18.25176868561973720 ) ) ;
#2373 = CARTESIAN_POINT ( 'NONE',  ( 2.450000000000000178, 0.000000000000000000, -0.3851141460153411078 ) ) ;
#2374 = VECTOR ( 'NONE', #5323, 1000.000000000000000 ) ;
#2375 = CARTESIAN_POINT ( 'NONE',  ( -80.00000000000002842, 50.75735931288069480, 4.242644059037076865 ) ) ;
#2376 = CARTESIAN_POINT ( 'NONE',  ( -17.91582325644631268, 61.21604956945397902, 3.318707400256076134 ) ) ;
#2377 = VERTEX_POINT ( 'NONE', #9184 ) ;
#2378 = CARTESIAN_POINT ( 'NONE',  ( -26.94161418247137263, 38.68192823000178038, 13.40559829713685502 ) ) ;
#2379 = CARTESIAN_POINT ( 'NONE',  ( 4.329456757236127551, 33.97246960341611555, -0.0004353087921988608999 ) ) ;
#2380 = CARTESIAN_POINT ( 'NONE',  ( 0.000000000000000000, 0.000000000000000000, -2.103846626247716234 ) ) ;
#2381 = CARTESIAN_POINT ( 'NONE',  ( -75.87500000204838102, 80.81189881250000440, 10.69163855873948243 ) ) ;
#2382 = DIRECTION ( 'NONE',  ( 0.8191520442889885789, 0.000000000000000000, 0.5735764363510507113 ) ) ;
#2383 = CARTESIAN_POINT ( 'NONE',  ( -76.25000000204838102, 65.69163855873948421, -25.81189881250000440 ) ) ;
#2384 = VERTEX_POINT ( 'NONE', #9244 ) ;
#2385 = CARTESIAN_POINT ( 'NONE',  ( -74.75000000409677625, 30.00000000000000355, 4.592425496802573578E-15 ) ) ;
#2386 = DIRECTION ( 'NONE',  ( -1.000000000000000000, -0.000000000000000000, -0.000000000000000000 ) ) ;
#2387 = CARTESIAN_POINT ( 'NONE',  ( -71.84375000409677625, 30.00000000000001421, 10.35533905932739174 ) ) ;
#2388 = AXIS2_PLACEMENT_3D ( 'NONE', #9667, #8055, #4404 ) ;
#2389 = CARTESIAN_POINT ( 'NONE',  ( -6.214759040711413718, 65.81103152010582846, -18.03762937187994453 ) ) ;
#2390 = CARTESIAN_POINT ( 'NONE',  ( -77.65625000204838102, 80.81189881250000440, -1.580522963032174394E-15 ) ) ;
#2391 = CARTESIAN_POINT ( 'NONE',  ( -78.00000000000001421, 59.24264068711928388, -11.22791868944003824 ) ) ;
#2392 = EDGE_CURVE ( 'NONE', #10874, #8848, #5605, .T. ) ;
#2393 = LINE ( 'NONE', #6068, #11623 ) ;
#2394 = CARTESIAN_POINT ( 'NONE',  ( -75.21875000409677625, 65.35533905932737753, 24.99999999999999645 ) ) ;
#2395 = AXIS2_PLACEMENT_3D ( 'NONE', #7305, #1952, #9203 ) ;
#2396 = CARTESIAN_POINT ( 'NONE',  ( 6.123233995736766282E-16, -30.00000000000000000, 5.000000000000000000 ) ) ;
#2397 = ADVANCED_FACE ( 'NONE', ( #8346 ), #130, .F. ) ;
#2398 = CARTESIAN_POINT ( 'NONE',  ( -72.96875000000000000, 30.00000000000001421, 10.35533905932739174 ) ) ;
#2399 = CARTESIAN_POINT ( 'NONE',  ( -80.00000000000001421, 71.97056274847716395, -1.499996628082204797 ) ) ;
#2400 = EDGE_LOOP ( 'NONE', ( #6141, #5251 ) ) ;
#2401 = CARTESIAN_POINT ( 'NONE',  ( 36.99999999999999289, 55.00000000000000000, 0.000000000000000000 ) ) ;
#2402 = EDGE_LOOP ( 'NONE', ( #591, #1737 ) ) ;
#2403 = ADVANCED_FACE ( 'NONE', ( #3794 ), #10198, .T. ) ;
#2404 = CARTESIAN_POINT ( 'NONE',  ( -64.55652465667151318, 48.91659104782370804, 3.512441407871431664 ) ) ;
#2405 = CARTESIAN_POINT ( 'NONE',  ( -78.87500000409677625, 55.00000000000000000, -24.99999999999999645 ) ) ;
#2406 = DIRECTION ( 'NONE',  ( -1.000000000000000000, -0.000000000000000000, -0.000000000000000000 ) ) ;
#2407 = VECTOR ( 'NONE', #8603, 1000.000000000000227 ) ;
#2408 = CARTESIAN_POINT ( 'NONE',  ( 12.85511924628072755, 70.12525320288015962, 15.98407836417939443 ) ) ;
#2409 = DIRECTION ( 'NONE',  ( -1.000000000000000000, -0.000000000000000000, -0.000000000000000000 ) ) ;
#2410 = ORIENTED_EDGE ( 'NONE', *, *, #8591, .F. ) ;
#2411 = CONICAL_SURFACE ( 'NONE', #10624, 2.500000000000000000, 0.9599310885968755924 ) ;
#2412 = CARTESIAN_POINT ( 'NONE',  ( -77.18750000204839523, 65.69163855873949842, 25.81189881250000440 ) ) ;
#2413 = ADVANCED_BREP_SHAPE_REPRESENTATION ( '', ( #684, #4738 ), #7754 ) ;
#2414 = DIRECTION ( 'NONE',  ( 0.000000000000000000, 0.000000000000000000, 1.000000000000000000 ) ) ;
#2415 = VECTOR ( 'NONE', #6695, 1000.000000000000000 ) ;
#2416 = EDGE_CURVE ( 'NONE', #10654, #69, #1093, .T. ) ;
#2417 = CARTESIAN_POINT ( 'NONE',  ( -80.00000000000002842, 54.99999999999998579, 8.485284746156354529 ) ) ;
#2418 = CARTESIAN_POINT ( 'NONE',  ( 5.576336621552477446, 55.00935349608988645, 0.004200982382114487428 ) ) ;
#2419 = DIRECTION ( 'NONE',  ( 1.000000000000000000, 0.000000000000000000, 0.000000000000000000 ) ) ;
#2420 = CYLINDRICAL_SURFACE ( 'NONE', #2995, 1.499999999999999556 ) ;
#2421 = PRESENTATION_LAYER_ASSIGNMENT (  '', '', ( #7397 ) ) ;
#2422 = ORIENTED_EDGE ( 'NONE', *, *, #9932, .F. ) ;
#2423 = CARTESIAN_POINT ( 'NONE',  ( -78.00000000000002842, 42.27207793864211283, -2.742637315201478909 ) ) ;
#2424 = ADVANCED_FACE ( 'NONE', ( #68 ), #11088, .F. ) ;
#2425 = CARTESIAN_POINT ( 'NONE',  ( -13.52239577877046095, 75.98118489547775312, -2.745668029642679642 ) ) ;
#2426 = EDGE_CURVE ( 'NONE', #5005, #7264, #6502, .T. ) ;
#2427 = ORIENTED_EDGE ( 'NONE', *, *, #2426, .T. ) ;
#2428 = CARTESIAN_POINT ( 'NONE',  ( -28.27494751366310766, 38.68366524674433293, 13.40386163033813460 ) ) ;
#2429 = CARTESIAN_POINT ( 'NONE',  ( -7.369671227794407642, 59.71994724795483478, -13.19184786971608858 ) ) ;
#2430 = CARTESIAN_POINT ( 'NONE',  ( -76.90625000204838102, 29.18810118750000271, 4.741568889096522788E-15 ) ) ;
#2431 = CIRCLE ( 'NONE', #6849, 4.999999999999997335 ) ;
#2432 = VECTOR ( 'NONE', #8895, 1000.000000000000000 ) ;
#2433 = ORIENTED_EDGE ( 'NONE', *, *, #11406, .T. ) ;
#2434 = CARTESIAN_POINT ( 'NONE',  ( -77.37500000204838102, 65.69163855873949842, 25.81189881250000440 ) ) ;
#2435 = DIRECTION ( 'NONE',  ( -1.000000000000000000, -0.000000000000000000, -0.000000000000000000 ) ) ;
#2436 = EDGE_CURVE ( 'NONE', #2740, #5005, #604, .T. ) ;
#2437 = ORIENTED_EDGE ( 'NONE', *, *, #10541, .F. ) ;
#2438 = DIRECTION ( 'NONE',  ( 0.000000000000000000, 0.000000000000000000, 1.000000000000000000 ) ) ;
#2439 = CIRCLE ( 'NONE', #3392, 1.500000000000001332 ) ;
#2440 = LINE ( 'NONE', #6225, #7415 ) ;
#2441 = CARTESIAN_POINT ( 'NONE',  ( -56.12525174590880539, 60.62665842901460422, 4.172128455226769006 ) ) ;
#2442 =( GEOMETRIC_REPRESENTATION_CONTEXT ( 3 ) GLOBAL_UNCERTAINTY_ASSIGNED_CONTEXT ( ( #4959 ) ) GLOBAL_UNIT_ASSIGNED_CONTEXT ( ( #4474, #11033, #983 ) ) REPRESENTATION_CONTEXT ( 'NONE', 'WORKASPACE' ) );
#2443 = VERTEX_POINT ( 'NONE', #10603 ) ;
#2444 = CARTESIAN_POINT ( 'NONE',  ( 18.14435054219095633, 65.56481479683655778, 18.33023711405786926 ) ) ;
#2445 = CARTESIAN_POINT ( 'NONE',  ( 8.189038476963473201, 38.19597440261895827, 12.92108669627241646 ) ) ;
#2446 = LINE ( 'NONE', #8084, #6790 ) ;
#2447 = DIRECTION ( 'NONE',  ( -0.000000000000000000, -0.000000000000000000, 1.000000000000000000 ) ) ;
#2448 = CARTESIAN_POINT ( 'NONE',  ( -75.50000000204840944, 44.30836144126053000, 25.81189881250000795 ) ) ;
#2449 = ORIENTED_EDGE ( 'NONE', *, *, #10815, .F. ) ;
#2450 = CARTESIAN_POINT ( 'NONE',  ( -74.65625000409679046, 30.00000000000000355, -10.35533905932738108 ) ) ;
#2451 = CARTESIAN_POINT ( 'NONE',  ( -80.00000000000002842, 59.24264068711927678, 14.22792543327563131 ) ) ;
#2452 = CARTESIAN_POINT ( 'NONE',  ( -67.56971494453328830, 50.00000002031717372, -0.0004507456344833478141 ) ) ;
#2453 = AXIS2_PLACEMENT_3D ( 'NONE', #9470, #1017, #5831 ) ;
#2454 = CARTESIAN_POINT ( 'NONE',  ( 17.18896242946999919, 60.50854855881860317, 20.47421955154796436 ) ) ;
#2455 = ORIENTED_EDGE ( 'NONE', *, *, #2058, .T. ) ;
#2456 = CARTESIAN_POINT ( 'NONE',  ( -77.28125000204838102, 55.00000000000000000, 25.81189881249999729 ) ) ;
#2457 = CARTESIAN_POINT ( 'NONE',  ( 36.99999999999999289, 55.00000000000000000, 0.000000000000000000 ) ) ;
#2458 = CARTESIAN_POINT ( 'NONE',  ( -78.00000000000002842, 46.51471862576140381, 9.985284746156354529 ) ) ;
#2459 = CARTESIAN_POINT ( 'NONE',  ( -39.18898618735786243, 44.43394377878069434, -18.33326528472845141 ) ) ;
#2460 = DIRECTION ( 'NONE',  ( -0.000000000000000000, -1.000000000000000000, -0.000000000000000000 ) ) ;
#2461 = CARTESIAN_POINT ( 'NONE',  ( -72.12500000000000000, 80.00000000000000000, -1.530808498934191324E-15 ) ) ;
#2462 = DIRECTION ( 'NONE',  ( -1.000000000000000000, -0.000000000000000000, -0.000000000000000000 ) ) ;
#2463 = EDGE_LOOP ( 'NONE', ( #3668, #6876 ) ) ;
#2464 = DIRECTION ( 'NONE',  ( -1.000000000000000000, -0.000000000000000000, -0.000000000000000000 ) ) ;
#2465 = PRODUCT_DEFINITION_CONTEXT ( 'detailed design', #5550, 'design' ) ;
#2466 = ORIENTED_EDGE ( 'NONE', *, *, #2980, .T. ) ;
#2467 = VECTOR ( 'NONE', #4475, 1000.000000000000000 ) ;
#2468 = CARTESIAN_POINT ( 'NONE',  ( -54.83316724383741558, 58.91257860089942255, 5.849939449132066649 ) ) ;
#2469 = PLANE ( 'NONE',  #9776 ) ;
#2470 = CARTESIAN_POINT ( 'NONE',  ( -15.09523335307150838, 60.00000000000000000, 4.640896189903090912E-12 ) ) ;
#2471 = DIRECTION ( 'NONE',  ( 1.000000000000000000, 6.033820786006286457E-17, -0.000000000000000000 ) ) ;
#2472 = CARTESIAN_POINT ( 'NONE',  ( 7.639074212767907213, 67.00087384642168331, -18.44261089144852050 ) ) ;
#2473 = AXIS2_PLACEMENT_3D ( 'NONE', #10582, #4368, #2511 ) ;
#2474 = CARTESIAN_POINT ( 'NONE',  ( -74.37500000204838102, 65.69163855873949842, 25.81189881250000084 ) ) ;
#2475 = AXIS2_PLACEMENT_3D ( 'NONE', #185, #10586, #1435 ) ;
#2476 = ORIENTED_EDGE ( 'NONE', *, *, #2126, .T. ) ;
#2477 = CARTESIAN_POINT ( 'NONE',  ( -75.96875000204839523, 80.81189881250000440, -1.580522963032174394E-15 ) ) ;
#2478 = CARTESIAN_POINT ( 'NONE',  ( 9.999999999999994671, -24.99999999999999645, -10.00000000000000000 ) ) ;
#2479 = UNCERTAINTY_MEASURE_WITH_UNIT (LENGTH_MEASURE( 1.000000000000000082E-05 ), #11367, 'distance_accuracy_value', 'NONE');
#2480 = EDGE_CURVE ( 'NONE', #6241, #1033, #2305, .T. ) ;
#2481 = CARTESIAN_POINT ( 'NONE',  ( -80.00000000000000000, 55.00000000000000000, -21.50000000000000000 ) ) ;
#2482 = CARTESIAN_POINT ( 'NONE',  ( -20.09713505253791865, 55.00123338473885326, -0.01962842282139863267 ) ) ;
#2483 = CIRCLE ( 'NONE', #8034, 1.500000000000001332 ) ;
#2484 =( NAMED_UNIT ( * ) PLANE_ANGLE_UNIT ( ) SI_UNIT ( $, .RADIAN. ) );
#2485 = AXIS2_PLACEMENT_3D ( 'NONE', #102, #7322, #8321 ) ;
#2486 = CARTESIAN_POINT ( 'NONE',  ( -75.00000000000000000, 29.76427645923893550, -3.754450393707159161 ) ) ;
#2487 = ORIENTED_EDGE ( 'NONE', *, *, #3740, .T. ) ;
#2488 = DIRECTION ( 'NONE',  ( 0.000000000000000000, 0.000000000000000000, 1.000000000000000000 ) ) ;
#2489 = CARTESIAN_POINT ( 'NONE',  ( -78.00000000000001421, 63.48528137423857487, 8.485284746156350977 ) ) ;
#2490 = ORIENTED_EDGE ( 'NONE', *, *, #5858, .F. ) ;
#2491 = CARTESIAN_POINT ( 'NONE',  ( -19.21475903476782676, 67.52694740698208875, 16.89034408144044264 ) ) ;
#2492 = CARTESIAN_POINT ( 'NONE',  ( -13.12707293678424136, 68.65161204859832367, -3.672914953887924661 ) ) ;
#2493 = CARTESIAN_POINT ( 'NONE',  ( -76.81250000204838102, 29.18810118750000626, -10.69163855873949309 ) ) ;
#2494 = AXIS2_PLACEMENT_3D ( 'NONE', #8818, #2462, #8757 ) ;
#2495 = ORIENTED_EDGE ( 'NONE', *, *, #4330, .T. ) ;
#2496 =( BOUNDED_CURVE ( )  B_SPLINE_CURVE ( 2, ( #2534, #2593, #2767, #10059, #10903, #51, #8945, #1797, #3492 ),
 .UNSPECIFIED., .F., .T. ) 
 B_SPLINE_CURVE_WITH_KNOTS ( ( 3, 2, 2, 2, 3 ),
 ( 0.1584082455038353654, 0.1782132311131151281, 0.1980182167223948908, 0.2178232023316745980, 0.2376281879409543607 ),
 .UNSPECIFIED. ) 
 CURVE ( )  GEOMETRIC_REPRESENTATION_ITEM ( )  RATIONAL_B_SPLINE_CURVE ( ( 1.000000000000020650, 0.9238795325112661994, 1.000000000000000000, 0.9238795325112868495, 1.000000000000000000, 0.9238795325112868495, 1.000000000000000000, 0.9238795325112363344, 1.000000000000050404 ) ) 
 REPRESENTATION_ITEM ( '' )  );
#2497 = CARTESIAN_POINT ( 'NONE',  ( -78.40625000204838102, 29.18810118750000271, 4.741568889096522788E-15 ) ) ;
#2498 = DIRECTION ( 'NONE',  ( -0.8191520442889974607, 0.000000000000000000, -0.5735764363510379438 ) ) ;
#2499 = SHAPE_REPRESENTATION_RELATIONSHIP ( 'NONE' , 'NONE' ,  #423, #9980 ) ;
#2500 = EDGE_CURVE ( 'NONE', #1770, #69, #9008, .T. ) ;
#2501 = CIRCLE ( 'NONE', #2698, 1.500000000000001332 ) ;
#2502 = DIRECTION ( 'NONE',  ( -1.000000000000000000, 0.000000000000000000, 0.000000000000000000 ) ) ;
#2503 = CARTESIAN_POINT ( 'NONE',  ( 22.64121015219242139, 59.33611995765907920, 2.510795356531756894 ) ) ;
#2504 = CARTESIAN_POINT ( 'NONE',  ( -21.41713453776156939, 58.30068857233666790, 6.174842648405145518 ) ) ;
#2505 = EDGE_LOOP ( 'NONE', ( #5491, #4064 ) ) ;
#2506 = CARTESIAN_POINT ( 'NONE',  ( -6.596024235661785085, 64.91289939244650498, -18.55097902119702624 ) ) ;
#2507 = CIRCLE ( 'NONE', #10717, 1.500000000000001332 ) ;
#2508 = CARTESIAN_POINT ( 'NONE',  ( -80.00000000000002842, 54.99999999999998579, 16.97056612039490986 ) ) ;
#2509 = PLANE ( 'NONE',  #7169 ) ;
#2510 = EDGE_CURVE ( 'NONE', #4836, #2315, #8236, .T. ) ;
#2511 = DIRECTION ( 'NONE',  ( 0.000000000000000000, 1.000000000000000000, 0.000000000000000000 ) ) ;
#2512 = CARTESIAN_POINT ( 'NONE',  ( -71.40810441781462714, 80.81189881250000440, 6.916273779317701376 ) ) ;
#2513 = AXIS2_PLACEMENT_3D ( 'NONE', #10407, #8446, #1063 ) ;
#2514 = EDGE_LOOP ( 'NONE', ( #3420, #232 ) ) ;
#2515 = CARTESIAN_POINT ( 'NONE',  ( -71.65625000409677625, 30.00000000000000355, -10.35533905932738108 ) ) ;
#2516 = LINE ( 'NONE', #5154, #5165 ) ;
#2517 = CARTESIAN_POINT ( 'NONE',  ( -64.85481352702973368, 50.50649124814121649, 2.217451826950856297 ) ) ;
#2518 = CARTESIAN_POINT ( 'NONE',  ( 11.81093755974026394, 42.10901286868706705, 16.77394813616862734 ) ) ;
#2519 = ORIENTED_EDGE ( 'NONE', *, *, #426, .T. ) ;
#2520 = DIRECTION ( 'NONE',  ( 0.000000000000000000, 0.000000000000000000, 1.000000000000000000 ) ) ;
#2521 = EDGE_CURVE ( 'NONE', #7145, #10896, #5093, .T. ) ;
#2522 = CARTESIAN_POINT ( 'NONE',  ( -59.04091006144056308, 57.21723975501232218, 4.493613460639234169 ) ) ;
#2523 = DIRECTION ( 'NONE',  ( -1.000000000000000000, -0.000000000000000000, -0.000000000000000000 ) ) ;
#2524 = CARTESIAN_POINT ( 'NONE',  ( 10.18651522171044554, 52.78500897206648546, 4.494612666729983275 ) ) ;
#2525 = CARTESIAN_POINT ( 'NONE',  ( -78.00000000000002842, 50.75735931288069480, 12.72792543327563131 ) ) ;
#2526 = CARTESIAN_POINT ( 'NONE',  ( -76.25000000204838102, 80.81189881250001861, -10.69163855873949132 ) ) ;
#2527 = DIRECTION ( 'NONE',  ( -1.000000000000000000, -0.000000000000000000, -0.000000000000000000 ) ) ;
#2528 = VERTEX_POINT ( 'NONE', #1687 ) ;
#2529 = DIRECTION ( 'NONE',  ( -1.000000000000000000, -6.033820786006286457E-17, -0.000000000000000000 ) ) ;
#2530 = ORIENTED_EDGE ( 'NONE', *, *, #5259, .F. ) ;
#2531 = CARTESIAN_POINT ( 'NONE',  ( -39.37536695926829111, 54.65609681119118335, -6.991488595795473771 ) ) ;
#2532 = PLANE ( 'NONE',  #10533 ) ;
#2533 = CARTESIAN_POINT ( 'NONE',  ( -78.87500000000002842, 30.00000000000003553, 4.592425496802568845E-15 ) ) ;
#2534 = CARTESIAN_POINT ( 'NONE',  ( -78.50000000000000000, 55.00000000000000000, -24.99999999999999645 ) ) ;
#2535 = CARTESIAN_POINT ( 'NONE',  ( -71.84375000204838102, 73.25176868561975141, -18.25176868561974430 ) ) ;
#2536 = EDGE_LOOP ( 'NONE', ( #8622, #1783, #1574, #5536 ) ) ;
#2537 = CARTESIAN_POINT ( 'NONE',  ( -78.00000000000002842, 42.27207793864211283, 2.742644059037075976 ) ) ;
#2538 = CARTESIAN_POINT ( 'NONE',  ( -76.81250000204839523, 29.18810118750000981, 10.69163855873950020 ) ) ;
#2539 = DIRECTION ( 'NONE',  ( -1.000000000000000000, 0.000000000000000000, 0.000000000000000000 ) ) ;
#2540 = LINE ( 'NONE', #787, #10162 ) ;
#2541 = CARTESIAN_POINT ( 'NONE',  ( 1.092736580689907200, 55.00849556027373666, 0.02481302773033131764 ) ) ;
#2542 = SURFACE_STYLE_FILL_AREA ( #9722 ) ;
#2543 = CARTESIAN_POINT ( 'NONE',  ( -75.00000000000000000, 30.11944236376617567, -5.798191608586254375 ) ) ;
#2544 = ORIENTED_EDGE ( 'NONE', *, *, #4268, .T. ) ;
#2545 = CARTESIAN_POINT ( 'NONE',  ( -78.00000000000002842, 46.51471862576140381, 3.371917798797308130E-06 ) ) ;
#2546 = PLANE ( 'NONE',  #1155 ) ;
#2547 = ORIENTED_EDGE ( 'NONE', *, *, #438, .F. ) ;
#2548 = CARTESIAN_POINT ( 'NONE',  ( -54.78543919591579225, 71.88463165892282802, 12.52160998826382965 ) ) ;
#2549 = CARTESIAN_POINT ( 'NONE',  ( -48.12707312818091765, 66.20688134294232441, -8.617576982512209938 ) ) ;
#2550 = DIRECTION ( 'NONE',  ( -1.000000000000000000, 0.000000000000000000, 0.000000000000000000 ) ) ;
#2551 = ORIENTED_EDGE ( 'NONE', *, *, #7785, .T. ) ;
#2552 = CARTESIAN_POINT ( 'NONE',  ( 0.000000000000000000, 110.0000000000000000, 0.000000000000000000 ) ) ;
#2553 = SURFACE_STYLE_FILL_AREA ( #3389 ) ;
#2554 = EDGE_CURVE ( 'NONE', #9492, #1807, #7105, .T. ) ;
#2555 = EDGE_CURVE ( 'NONE', #3874, #7344, #10782, .T. ) ;
#2556 = ORIENTED_EDGE ( 'NONE', *, *, #9539, .T. ) ;
#2557 = DIRECTION ( 'NONE',  ( -1.000000000000000000, -0.000000000000000000, -0.000000000000000000 ) ) ;
#2558 = DIRECTION ( 'NONE',  ( 0.8191520442889974607, 1.003171929053531649E-16, -0.5735764363510379438 ) ) ;
#2559 = CARTESIAN_POINT ( 'NONE',  ( 14.24053855247502121, 55.00473321740069821, 0.01576102579767488590 ) ) ;
#2560 = EDGE_LOOP ( 'NONE', ( #601, #10241, #3736, #906 ) ) ;
#2561 = CARTESIAN_POINT ( 'NONE',  ( -6.881425704338284710, 65.81090974167105401, -18.03733726640467694 ) ) ;
#2562 = CARTESIAN_POINT ( 'NONE',  ( -19.88142569839470042, 67.52672413929985851, 16.89011978890229315 ) ) ;
#2563 = DIRECTION ( 'NONE',  ( -1.000000000000000000, -0.000000000000000000, -0.000000000000000000 ) ) ;
#2564 = DIRECTION ( 'NONE',  ( -1.000000000000000000, 0.000000000000000000, 0.000000000000000000 ) ) ;
#2565 = AXIS2_PLACEMENT_3D ( 'NONE', #6837, #11414, #3892 ) ;
#2566 = DIRECTION ( 'NONE',  ( 0.000000000000000000, 1.000000000000000000, 0.000000000000000000 ) ) ;
#2567 = ORIENTED_EDGE ( 'NONE', *, *, #3528, .F. ) ;
#2568 = CARTESIAN_POINT ( 'NONE',  ( -71.75000000409677625, 30.00000000000000355, 4.592425496802573578E-15 ) ) ;
#2569 = DIRECTION ( 'NONE',  ( 0.000000000000000000, 0.000000000000000000, -1.000000000000000000 ) ) ;
#2570 = CARTESIAN_POINT ( 'NONE',  ( -72.12500000409677625, 55.00000000000000000, 24.99999999999999645 ) ) ;
#2571 = EDGE_CURVE ( 'NONE', #6608, #1419, #8825, .T. ) ;
#2572 = EDGE_CURVE ( 'NONE', #7093, #8959, #7760, .T. ) ;
#2573 = CARTESIAN_POINT ( 'NONE',  ( -62.51030605291772702, 43.28161195024001273, 17.55542603392786916 ) ) ;
#2574 = EDGE_CURVE ( 'NONE', #656, #3299, #5189, .T. ) ;
#2575 = VERTEX_POINT ( 'NONE', #7101 ) ;
#2576 = CARTESIAN_POINT ( 'NONE',  ( 53.00000000000000000, 51.46446609406726935, -3.535533905932738197 ) ) ;
#2577 = LINE ( 'NONE', #707, #115 ) ;
#2578 = VERTEX_POINT ( 'NONE', #6201 ) ;
#2579 = CARTESIAN_POINT ( 'NONE',  ( -80.00000000000000000, 55.00000000000000000, -24.99999999999999645 ) ) ;
#2580 = EDGE_CURVE ( 'NONE', #6077, #2686, #10144, .T. ) ;
#2581 = ADVANCED_FACE ( 'NONE', ( #1123 ), #5007, .F. ) ;
#2582 = CARTESIAN_POINT ( 'NONE',  ( 12.51356687061732664, 54.66830098263688598, 4.999997770403642683 ) ) ;
#2583 = CARTESIAN_POINT ( 'NONE',  ( -79.43750000204838102, 65.69163855873948421, -25.81189881250000440 ) ) ;
#2584 = DIRECTION ( 'NONE',  ( 0.000000000000000000, 1.000000000000000000, 0.000000000000000000 ) ) ;
#2585 = ORIENTED_EDGE ( 'NONE', *, *, #3159, .T. ) ;
#2586 = EDGE_CURVE ( 'NONE', #10642, #9073, #399, .T. ) ;
#2587 = CARTESIAN_POINT ( 'NONE',  ( -78.00000000000001421, 67.72792206135787296, 4.242644059037073312 ) ) ;
#2588 = ORIENTED_EDGE ( 'NONE', *, *, #8050, .F. ) ;
#2589 = CARTESIAN_POINT ( 'NONE',  ( 19.98279345720612454, 75.57879140538503293, 14.21315688551485579 ) ) ;
#2590 = CARTESIAN_POINT ( 'NONE',  ( 7.836421160393130414, 41.20749391036343212, 2.739689159572535448 ) ) ;
#2591 = CARTESIAN_POINT ( 'NONE',  ( 2.500000000000000000, 0.000000000000000000, -2.267810516609437776 ) ) ;
#2592 = COLOUR_RGB ( '',0.8941176470588234615, 0.8941176470588234615, 0.8941176470588234615 ) ;
#2593 = CARTESIAN_POINT ( 'NONE',  ( -78.40625000000005684, 65.35533905932518906, -25.00000000000207478 ) ) ;
#2594 = CARTESIAN_POINT ( 'NONE',  ( -73.62500000204838102, 44.30836144126049447, -25.81189881249999019 ) ) ;
#2595 = VERTEX_POINT ( 'NONE', #11238 ) ;
#2596 = CARTESIAN_POINT ( 'NONE',  ( -76.53125000204839523, 36.74823131438024859, -18.25176868561973720 ) ) ;
#2597 = LINE ( 'NONE', #5241, #1541 ) ;
#2598 = DIRECTION ( 'NONE',  ( -0.000000000000000000, -0.000000000000000000, -1.000000000000000000 ) ) ;
#2599 = CARTESIAN_POINT ( 'NONE',  ( -57.99733838118905282, 54.99932032637487112, 0.003899505293572518017 ) ) ;
#2600 = CARTESIAN_POINT ( 'NONE',  ( 0.000000000000000000, 0.000000000000000000, 0.000000000000000000 ) ) ;
#2601 = CARTESIAN_POINT ( 'NONE',  ( -5.000000000000000000, -2.886751345948134428, -5.653418012614792154 ) ) ;
#2602 = VECTOR ( 'NONE', #5265, 1000.000000000000000 ) ;
#2603 = VERTEX_POINT ( 'NONE', #8563 ) ;
#2604 = CARTESIAN_POINT ( 'NONE',  ( -19.92923235869172061, 55.82034979468773628, 4.934922690953704283 ) ) ;
#2605 = FACE_OUTER_BOUND ( 'NONE', #8879, .T. ) ;
#2606 = EDGE_LOOP ( 'NONE', ( #6377, #11266 ) ) ;
#2607 = CARTESIAN_POINT ( 'NONE',  ( -55.07084767368650091, 71.24562247638961310, 13.33442519937083404 ) ) ;
#2608 = CARTESIAN_POINT ( 'NONE',  ( -75.59375000204839523, 36.74823131438026280, 18.25176868561974786 ) ) ;
#2609 = CONICAL_SURFACE ( 'NONE', #7769, 17.04557674096337649, 0.1745329251994333364 ) ;
#2610 = VERTEX_POINT ( 'NONE', #10169 ) ;
#2611 = CARTESIAN_POINT ( 'NONE',  ( -74.93750000204839523, 65.69163855873948421, -25.81189881250000440 ) ) ;
#2612 = LINE ( 'NONE', #11465, #1821 ) ;
#2613 = EDGE_CURVE ( 'NONE', #3954, #2110, #5571, .T. ) ;
#2614 = CARTESIAN_POINT ( 'NONE',  ( -80.00000000000002842, 42.27207793864211283, -4.242637315201479353 ) ) ;
#2615 = CARTESIAN_POINT ( 'NONE',  ( 21.86348472080128502, 58.97384788876435380, 3.051976829295043103 ) ) ;
#2616 = CARTESIAN_POINT ( 'NONE',  ( -61.37538809735546863, 55.34397181478555439, 6.994694612480975238 ) ) ;
#2617 = EDGE_LOOP ( 'NONE', ( #462, #2641, #2728, #1647 ) ) ;
#2618 = CARTESIAN_POINT ( 'NONE',  ( -63.06671435217206323, 41.62111505249539078, 16.30162306856191989 ) ) ;
#2619 = VECTOR ( 'NONE', #11191, 1000.000000000000000 ) ;
#2620 = CARTESIAN_POINT ( 'NONE',  ( -40.60828084101493829, 48.86090744392433294, -20.20262880343927847 ) ) ;
#2621 = DIRECTION ( 'NONE',  ( 0.000000000000000000, 0.9848077530122080203, 0.1736481776669307198 ) ) ;
#2622 = VECTOR ( 'NONE', #2700, 1000.000000000000114 ) ;
#2623 = DIRECTION ( 'NONE',  ( 0.000000000000000000, 0.000000000000000000, 1.000000000000000000 ) ) ;
#2624 = DIRECTION ( 'NONE',  ( -0.000000000000000000, 0.000000000000000000, -1.000000000000000000 ) ) ;
#2625 = ORIENTED_EDGE ( 'NONE', *, *, #9797, .F. ) ;
#2626 = DIRECTION ( 'NONE',  ( 1.000000000000000000, 6.033820786006286457E-17, 0.000000000000000000 ) ) ;
#2627 = DIRECTION ( 'NONE',  ( -0.000000000000000000, -0.000000000000000000, 1.000000000000000000 ) ) ;
#2628 = DIRECTION ( 'NONE',  ( 0.000000000000000000, 0.000000000000000000, 1.000000000000000000 ) ) ;
#2629 = CARTESIAN_POINT ( 'NONE',  ( -44.39182476880109363, 68.38060868816502591, -16.29271878486493463 ) ) ;
#2630 = AXIS2_PLACEMENT_3D ( 'NONE', #1301, #6948, #10456 ) ;
#2631 = ORIENTED_EDGE ( 'NONE', *, *, #9786, .T. ) ;
#2632 = CARTESIAN_POINT ( 'NONE',  ( -74.84375000000005684, 65.35533905932891230, 24.99999999999828404 ) ) ;
#2633 = CARTESIAN_POINT ( 'NONE',  ( -59.81854832799476185, 56.60795527072578182, 4.745860713526097285 ) ) ;
#2634 = ORIENTED_EDGE ( 'NONE', *, *, #6057, .F. ) ;
#2635 =( BOUNDED_CURVE ( )  B_SPLINE_CURVE ( 2, ( #815, #1832, #4598, #10938, #5444, #7190, #756, #4485, #9208 ),
 .UNSPECIFIED., .F., .T. ) 
 B_SPLINE_CURVE_WITH_KNOTS ( ( 3, 2, 2, 2, 3 ),
 ( 0.3168733201082642448, 0.3366713418703649596, 0.3564693636324655635, 0.3762673853945661673, 0.3960654071566668821 ),
 .UNSPECIFIED. ) 
 CURVE ( )  GEOMETRIC_REPRESENTATION_ITEM ( )  RATIONAL_B_SPLINE_CURVE ( ( 1.000000000000000000, 0.9238795325112868495, 1.000000000000000000, 0.9238795325112868495, 1.000000000000000000, 0.9238795325112868495, 1.000000000000000000, 0.9238795325112868495, 1.000000000000000000 ) ) 
 REPRESENTATION_ITEM ( '' )  );
#2636 = DIRECTION ( 'NONE',  ( 0.000000000000000000, 0.000000000000000000, 1.000000000000000000 ) ) ;
#2637 = CARTESIAN_POINT ( 'NONE',  ( -78.00000000000002842, 42.27207793864211283, 12.72792543327562775 ) ) ;
#2638 = CARTESIAN_POINT ( 'NONE',  ( -74.56250000204839523, 80.81189881250001861, 10.69163855873948599 ) ) ;
#2639 = CARTESIAN_POINT ( 'NONE',  ( -77.65625000204838102, 80.81189881250000440, -1.580522963032174394E-15 ) ) ;
#2640 = AXIS2_PLACEMENT_3D ( 'NONE', #11010, #113, #1136 ) ;
#2641 = ORIENTED_EDGE ( 'NONE', *, *, #3201, .T. ) ;
#2642 = CARTESIAN_POINT ( 'NONE',  ( -76.90625000204839523, 36.74823131438026280, 18.25176868561974786 ) ) ;
#2643 = VERTEX_POINT ( 'NONE', #2148 ) ;
#2644 = CARTESIAN_POINT ( 'NONE',  ( -7.287414961092598453, 58.76490461671014032, -3.306449428548710934 ) ) ;
#2645 = CARTESIAN_POINT ( 'NONE',  ( -14.92871872213861018, 67.42576808392385601, 6.633445025436828679 ) ) ;
#2646 = EDGE_CURVE ( 'NONE', #1761, #5798, #4042, .T. ) ;
#2647 = CARTESIAN_POINT ( 'NONE',  ( -77.18750000204839523, 65.69163855873949842, 25.81189881250000084 ) ) ;
#2648 = DIRECTION ( 'NONE',  ( -1.000000000000000000, -0.000000000000000000, -0.000000000000000000 ) ) ;
#2649 = AXIS2_PLACEMENT_3D ( 'NONE', #10829, #4493, #1611 ) ;
#2650 = FACE_OUTER_BOUND ( 'NONE', #2560, .T. ) ;
#2651 = CARTESIAN_POINT ( 'NONE',  ( -73.34375000204839523, 73.25176868561975141, -18.25176868561974430 ) ) ;
#2652 = EDGE_LOOP ( 'NONE', ( #9846, #6577, #4030, #3111 ) ) ;
#2653 = CYLINDRICAL_SURFACE ( 'NONE', #3545, 24.99999999999999645 ) ;
#2654 = CARTESIAN_POINT ( 'NONE',  ( -76.06250000409679046, 37.32233047033631124, -17.67766952966368166 ) ) ;
#2655 = EDGE_CURVE ( 'NONE', #11822, #9962, #4854, .T. ) ;
#2656 = CARTESIAN_POINT ( 'NONE',  ( -5.000000000000000000, 2.886751345948126879, -0.4465819873852047150 ) ) ;
#2657 = B_SPLINE_CURVE_WITH_KNOTS ( 'NONE', 3,
 ( #9833, #4390, #5057, #661 ),
 .UNSPECIFIED., .F., .F.,
 ( 4, 4 ),
 ( 0.000000000000000000, 1.000000000000000000 ),
 .UNSPECIFIED. ) ;
#2658 = CARTESIAN_POINT ( 'NONE',  ( -77.18750000409679046, 72.67766952966368876, -17.67766952966368876 ) ) ;
#2659 = CARTESIAN_POINT ( 'NONE',  ( -25.90292780145558282, 54.98522453252181919, 0.01301329896340179364 ) ) ;
#2660 = APPLICATION_PROTOCOL_DEFINITION ( 'draft international standard', 'automotive_design', 1998, #5793 ) ;
#2661 = CARTESIAN_POINT ( 'NONE',  ( -17.98788677490622234, 73.94881694393184546, -11.19406059795755226 ) ) ;
#2662 = CARTESIAN_POINT ( 'NONE',  ( -11.96064323986153255, 59.99999999999997868, 0.3308892280880238457 ) ) ;
#2663 = AXIS2_PLACEMENT_3D ( 'NONE', #5927, #7953, #9570 ) ;
#2664 = DIRECTION ( 'NONE',  ( 0.000000000000000000, -1.000000000000000000, 0.000000000000000000 ) ) ;
#2665 = B_SPLINE_CURVE_WITH_KNOTS ( 'NONE', 3,
 ( #6657, #7554, #407, #4974 ),
 .UNSPECIFIED., .F., .F.,
 ( 4, 4 ),
 ( 2.380735201027449880E-07, 0.002921158011986725936 ),
 .UNSPECIFIED. ) ;
#2666 = ORIENTED_EDGE ( 'NONE', *, *, #10956, .F. ) ;
#2667 = CARTESIAN_POINT ( 'NONE',  ( -37.81096152632984797, 42.07775575353442576, -16.80518334814213333 ) ) ;
#2668 = CARTESIAN_POINT ( 'NONE',  ( -77.09375000204839523, 36.74823131438026280, 18.25176868561974786 ) ) ;
#2669 = CIRCLE ( 'NONE', #7273, 1.500000000000001332 ) ;
#2670 = CIRCLE ( 'NONE', #362, 1.500000000000001332 ) ;
#2671 = EDGE_LOOP ( 'NONE', ( #8662, #1669, #10822, #1688 ) ) ;
#2672 = CARTESIAN_POINT ( 'NONE',  ( -76.62500000000005684, 79.99999999999991473, -1.530808498934185605E-15 ) ) ;
#2673 = CARTESIAN_POINT ( 'NONE',  ( -26.94161418247137263, 38.68192823000178038, 13.40559829713685502 ) ) ;
#2674 = FILL_AREA_STYLE ('',( #1816 ) ) ;
#2675 = EDGE_CURVE ( 'NONE', #11519, #9206, #2116, .T. ) ;
#2676 = ORIENTED_EDGE ( 'NONE', *, *, #8410, .T. ) ;
#2677 = CARTESIAN_POINT ( 'NONE',  ( 0.000000000000000000, 0.000000000000000000, 0.000000000000000000 ) ) ;
#2678 = CARTESIAN_POINT ( 'NONE',  ( -6.569594461653855078, 55.00124529901456327, -0.01228082968807806159 ) ) ;
#2679 = VECTOR ( 'NONE', #482, 1000.000000000000000 ) ;
#2680 = ORIENTED_EDGE ( 'NONE', *, *, #10681, .T. ) ;
#2681 = CARTESIAN_POINT ( 'NONE',  ( -65.17448922114576249, 36.67438677247554324, 10.54995967583099237 ) ) ;
#2682 = CARTESIAN_POINT ( 'NONE',  ( 3.737309610555803463, 34.06887424008940712, -2.059134394038261817 ) ) ;
#2683 = CARTESIAN_POINT ( 'NONE',  ( -78.00000000000001421, 67.72792206135787296, -11.22791868944004534 ) ) ;
#2684 = CYLINDRICAL_SURFACE ( 'NONE', #6703, 4.999999999999984013 ) ;
#2685 = CYLINDRICAL_SURFACE ( 'NONE', #4988, 1.500000000000001332 ) ;
#2686 = VERTEX_POINT ( 'NONE', #3947 ) ;
#2687 = CARTESIAN_POINT ( 'NONE',  ( -83.00000000000000000, 55.00000000000000000, 0.000000000000000000 ) ) ;
#2688 = CARTESIAN_POINT ( 'NONE',  ( -40.24052535843971867, 55.00473963081345374, 0.01574568287803283437 ) ) ;
#2689 = CARTESIAN_POINT ( 'NONE',  ( -62.51716279675893873, 51.69589315519270656, 3.766953055518623472 ) ) ;
#2690 = AXIS2_PLACEMENT_3D ( 'NONE', #5697, #5452, #9271 ) ;
#2691 = ORIENTED_EDGE ( 'NONE', *, *, #3208, .F. ) ;
#2692 = DIRECTION ( 'NONE',  ( 0.000000000000000000, 1.000000000000000000, 0.000000000000000000 ) ) ;
#2693 = EDGE_CURVE ( 'NONE', #11779, #3307, #4608, .T. ) ;
#2694 = VECTOR ( 'NONE', #615, 1000.000000000000000 ) ;
#2695 = CARTESIAN_POINT ( 'NONE',  ( -69.53699434246021838, 50.16068223471152265, 1.299115590555422139 ) ) ;
#2696 = ORIENTED_EDGE ( 'NONE', *, *, #11695, .T. ) ;
#2697 = CARTESIAN_POINT ( 'NONE',  ( 47.00000000000000000, 105.0000000000000142, 0.000000000000000000 ) ) ;
#2698 = AXIS2_PLACEMENT_3D ( 'NONE', #2960, #1031, #3679 ) ;
#2699 = CARTESIAN_POINT ( 'NONE',  ( 47.00000000000000000, 51.46446609406726935, -3.535533905932743526 ) ) ;
#2700 = DIRECTION ( 'NONE',  ( 0.9986295347545739443, 0.05233595624294401505, 0.000000000000000000 ) ) ;
#2701 = CARTESIAN_POINT ( 'NONE',  ( -74.09375000204839523, 36.74823131438026280, 18.25176868561974786 ) ) ;
#2702 = CARTESIAN_POINT ( 'NONE',  ( -77.37500000204838102, 65.69163855873949842, 25.81189881250000440 ) ) ;
#2703 = ORIENTED_EDGE ( 'NONE', *, *, #9671, .T. ) ;
#2704 = CARTESIAN_POINT ( 'NONE',  ( -75.40625000204839523, 36.74823131438026280, 18.25176868561974786 ) ) ;
#2705 = AXIS2_PLACEMENT_3D ( 'NONE', #6076, #10774, #8759 ) ;
#2706 = CIRCLE ( 'NONE', #10913, 24.99999999999999645 ) ;
#2707 = ORIENTED_EDGE ( 'NONE', *, *, #11755, .F. ) ;
#2708 = CARTESIAN_POINT ( 'NONE',  ( -4.954815148401325864, 57.21385113419372459, -4.495241971010075943 ) ) ;
#2709 = CARTESIAN_POINT ( 'NONE',  ( 1.206260390864687171, 46.37779328219373554, -11.21151207404757066 ) ) ;
#2710 = EDGE_CURVE ( 'NONE', #9787, #3028, #4226, .T. ) ;
#2711 = CARTESIAN_POINT ( 'NONE',  ( -75.21875000204839523, 29.18810118750000271, 4.741568889096522788E-15 ) ) ;
#2712 =( BOUNDED_CURVE ( )  B_SPLINE_CURVE ( 2, ( #9519, #8628, #10465, #3171, #6839, #11536, #5385, #9035, #812 ),
 .UNSPECIFIED., .F., .T. ) 
 B_SPLINE_CURVE_WITH_KNOTS ( ( 3, 2, 2, 2, 3 ),
 ( 0.3960654071566668821, 0.4158759072859738448, 0.4356864074152808075, 0.4554969075445878257, 0.4753074076738947884 ),
 .UNSPECIFIED. ) 
 CURVE ( )  GEOMETRIC_REPRESENTATION_ITEM ( )  RATIONAL_B_SPLINE_CURVE ( ( 1.000000000000000000, 0.9238795325112867385, 1.000000000000000000, 0.9238795325112867385, 1.000000000000000000, 0.9238795325112867385, 1.000000000000000000, 0.9238795325112889589, 0.9999999999999977796 ) ) 
 REPRESENTATION_ITEM ( '' )  );
#2713 = CARTESIAN_POINT ( 'NONE',  ( 1.653121499799245830, -4.819072548984015825, -6.048595712916167599 ) ) ;
#2714 = AXIS2_PLACEMENT_3D ( 'NONE', #875, #819, #2692 ) ;
#2715 = ORIENTED_EDGE ( 'NONE', *, *, #4119, .F. ) ;
#2716 = SURFACE_SIDE_STYLE ('',( #11227 ) ) ;
#2717 = CARTESIAN_POINT ( 'NONE',  ( -77.93750000409679046, 37.32233047033631124, 17.67766952966369232 ) ) ;
#2718 = DIRECTION ( 'NONE',  ( 0.000000000000000000, 0.000000000000000000, 1.000000000000000000 ) ) ;
#2719 =( REPRESENTATION_RELATIONSHIP ('NONE','NONE', #5489, #9454 ) REPRESENTATION_RELATIONSHIP_WITH_TRANSFORMATION ( #6434 )SHAPE_REPRESENTATION_RELATIONSHIP( ) );
#2720 = CARTESIAN_POINT ( 'NONE',  ( -33.09269368653934151, 54.97643580162243637, -0.01155639149150148627 ) ) ;
#2721 = APPLICATION_PROTOCOL_DEFINITION ( 'draft international standard', 'automotive_design', 1998, #20 ) ;
#2722 = CONICAL_SURFACE ( 'NONE', #6149, 5.000000000000000888, 1.047197551196596299 ) ;
#2723 = EDGE_CURVE ( 'NONE', #1879, #7325, #6538, .T. ) ;
#2724 = CARTESIAN_POINT ( 'NONE',  ( -21.66281002447331261, 76.95651461112846903, 1.430698443491871474 ) ) ;
#2725 = EDGE_CURVE ( 'NONE', #658, #7013, #7610, .T. ) ;
#2726 = B_SPLINE_CURVE_WITH_KNOTS ( 'NONE', 3,
 ( #10652, #3416, #6971, #9707 ),
 .UNSPECIFIED., .F., .F.,
 ( 4, 4 ),
 ( 0.0003222502065252045981, 0.003846531889534238625 ),
 .UNSPECIFIED. ) ;
#2727 = DIRECTION ( 'NONE',  ( 0.000000000000000000, 1.000000000000000000, 0.000000000000000000 ) ) ;
#2728 = ORIENTED_EDGE ( 'NONE', *, *, #6109, .F. ) ;
#2729 = PLANE ( 'NONE',  #7869 ) ;
#2730 = EDGE_LOOP ( 'NONE', ( #6514, #10020, #9547, #4423 ) ) ;
#2731 = CARTESIAN_POINT ( 'NONE',  ( -9.969360172258976860, 70.58303384883494402, -14.12411716821732277 ) ) ;
#2732 = CARTESIAN_POINT ( 'NONE',  ( -73.62500000204839523, 44.30836144126050158, -25.81189881249999374 ) ) ;
#2733 = EDGE_LOOP ( 'NONE', ( #5220, #4348, #8989, #5133 ) ) ;
#2734 = ADVANCED_FACE ( 'NONE', ( #9515 ), #7668, .F. ) ;
#2735 = CARTESIAN_POINT ( 'NONE',  ( -76.90625000000005684, 65.35533905932732068, -24.99999999999990052 ) ) ;
#2736 = CARTESIAN_POINT ( 'NONE',  ( -24.81096152833125856, 44.41791055217656492, 18.37268719335390443 ) ) ;
#2737 = EDGE_LOOP ( 'NONE', ( #1207, #1028, #1467, #536 ) ) ;
#2738 = CARTESIAN_POINT ( 'NONE',  ( -78.00000000000002842, 54.99999999999998579, 16.97056612039490986 ) ) ;
#2739 = CARTESIAN_POINT ( 'NONE',  ( -10.95223875328497343, 55.00428177097578697, -0.003223779858058093296 ) ) ;
#2740 = VERTEX_POINT ( 'NONE', #1241 ) ;
#2741 = CARTESIAN_POINT ( 'NONE',  ( -18.54809237114100284, 67.52717067466427636, 16.89056837398185351 ) ) ;
#2742 = CARTESIAN_POINT ( 'NONE',  ( -33.30269350532120143, 33.99387206627966407, -1.031609878214063025 ) ) ;
#2743 = CARTESIAN_POINT ( 'NONE',  ( 14.99999999999999645, 55.00000000000000000, -20.00000000000000000 ) ) ;
#2744 =( LENGTH_UNIT ( ) NAMED_UNIT ( * ) SI_UNIT ( .MILLI., .METRE. ) );
#2745 = DIRECTION ( 'NONE',  ( 1.000000000000000000, 0.000000000000000000, 0.000000000000000000 ) ) ;
#2746 = CARTESIAN_POINT ( 'NONE',  ( -3.000000000000000000, 0.000000000000000000, -2.617914285714285416 ) ) ;
#2747 = ORIENTED_EDGE ( 'NONE', *, *, #3301, .F. ) ;
#2748 = DIRECTION ( 'NONE',  ( 1.000000000000000000, 6.033820786006286457E-17, 0.000000000000000000 ) ) ;
#2749 = CARTESIAN_POINT ( 'NONE',  ( -35.16317177855322029, 54.99748849700297626, -0.0002045196618292968900 ) ) ;
#2750 = CARTESIAN_POINT ( 'NONE',  ( -45.01221456438528890, 58.97241515813631452, -3.054071859287629032 ) ) ;
#2751 = CARTESIAN_POINT ( 'NONE',  ( -77.65624999999998579, 44.64466094066740709, 24.99999999999465672 ) ) ;
#2752 = DIRECTION ( 'NONE',  ( -1.000000000000000000, 0.000000000000000000, 0.000000000000000000 ) ) ;
#2753 = EDGE_LOOP ( 'NONE', ( #1012, #5577 ) ) ;
#2754 = DIRECTION ( 'NONE',  ( -1.000000000000000000, -0.000000000000000000, -0.000000000000000000 ) ) ;
#2755 = DIRECTION ( 'NONE',  ( -1.000000000000000000, 0.000000000000000000, 0.000000000000000000 ) ) ;
#2756 = CARTESIAN_POINT ( 'NONE',  ( -66.47562283042974229, 38.19906477560226676, 12.92409071120044040 ) ) ;
#2757 = CARTESIAN_POINT ( 'NONE',  ( -4.655134714661222084, 66.15614397521940759, -22.37326029429084429 ) ) ;
#2758 = CARTESIAN_POINT ( 'NONE',  ( -76.25000000204838102, 80.81189881250001861, -10.69163855873949132 ) ) ;
#2759 = VERTEX_POINT ( 'NONE', #4071 ) ;
#2760 = CARTESIAN_POINT ( 'NONE',  ( -77.28125000204839523, 73.25176868561975141, 18.25176868561974075 ) ) ;
#2761 = ORIENTED_EDGE ( 'NONE', *, *, #4332, .T. ) ;
#2762 = CARTESIAN_POINT ( 'NONE',  ( 14.96838742389068244, 71.73858167410611486, 18.60395740379449947 ) ) ;
#2763 = CARTESIAN_POINT ( 'NONE',  ( -17.25615151965529037, 63.89925965980745559, 10.84111801642336026 ) ) ;
#2764 = CARTESIAN_POINT ( 'NONE',  ( -75.68750000204839523, 65.69163855873949842, 25.81189881250000084 ) ) ;
#2765 = EDGE_CURVE ( 'NONE', #1955, #364, #5771, .T. ) ;
#2766 = DIRECTION ( 'NONE',  ( 0.000000000000000000, 1.000000000000000000, 0.000000000000000000 ) ) ;
#2767 = CARTESIAN_POINT ( 'NONE',  ( -78.31250000000004263, 72.67766952966363192, -17.67766952966363903 ) ) ;
#2768 = VERTEX_POINT ( 'NONE', #1305 ) ;
#2769 = DIRECTION ( 'NONE',  ( -0.000000000000000000, -0.000000000000000000, -1.000000000000000000 ) ) ;
#2770 = CARTESIAN_POINT ( 'NONE',  ( -77.65625000409677625, 30.00000000000000355, -10.35533905932738108 ) ) ;
#2771 = ADVANCED_FACE ( 'NONE', ( #4729 ), #10343, .F. ) ;
#2772 = CARTESIAN_POINT ( 'NONE',  ( -80.00000000000001421, 67.72792206135787296, 12.72792543327562775 ) ) ;
#2773 = CARTESIAN_POINT ( 'NONE',  ( -39.04772848043890576, 54.99975663035424134, 0.008780986960116223677 ) ) ;
#2774 = EDGE_CURVE ( 'NONE', #9261, #3782, #8383, .T. ) ;
#2775 = AXIS2_PLACEMENT_3D ( 'NONE', #7736, #1865, #3788 ) ;
#2776 = CARTESIAN_POINT ( 'NONE',  ( -1.462190304540868846, 65.05665727266017484, -19.56733247748169191 ) ) ;
#2777 = LINE ( 'NONE', #10068, #5506 ) ;
#2778 = ORIENTED_EDGE ( 'NONE', *, *, #10548, .T. ) ;
#2779 = CARTESIAN_POINT ( 'NONE',  ( -78.00000000000001421, 46.51471862576140381, -6.985278002320760571 ) ) ;
#2780 = ORIENTED_EDGE ( 'NONE', *, *, #7328, .T. ) ;
#2781 = CARTESIAN_POINT ( 'NONE',  ( -4.188986194789085182, 52.25407379690145859, -20.98118322582191908 ) ) ;
#2782 = CARTESIAN_POINT ( 'NONE',  ( -71.53052368722832455, 77.35376350879521112, 12.90594348738575903 ) ) ;
#2783 = AXIS2_PLACEMENT_3D ( 'NONE', #5496, #9145, #3695 ) ;
#2784 = ORIENTED_EDGE ( 'NONE', *, *, #11012, .T. ) ;
#2785 = CARTESIAN_POINT ( 'NONE',  ( -73.06250000204840944, 80.81189881250001861, 10.69163855873948599 ) ) ;
#2786 = CARTESIAN_POINT ( 'NONE',  ( -40.33720992201957500, 55.00042869323097960, -21.02810349118288258 ) ) ;
#2787 = ORIENTED_EDGE ( 'NONE', *, *, #236, .F. ) ;
#2788 = ADVANCED_FACE ( 'NONE', ( #10228 ), #2609, .F. ) ;
#2789 = DIRECTION ( 'NONE',  ( 0.000000000000000000, 1.000000000000000000, 0.000000000000000000 ) ) ;
#2790 = CARTESIAN_POINT ( 'NONE',  ( 19.14436220527237253, 71.77763100192429135, 12.89423484158165500 ) ) ;
#2791 = AXIS2_PLACEMENT_3D ( 'NONE', #5976, #8955, #4402 ) ;
#2792 = ORIENTED_EDGE ( 'NONE', *, *, #4925, .T. ) ;
#2793 = CARTESIAN_POINT ( 'NONE',  ( -27.60828084806726324, 38.68279673837142241, 13.40472996373423520 ) ) ;
#2794 = CARTESIAN_POINT ( 'NONE',  ( -1.855729112296511385, 44.43418165317581980, -18.33336562707187412 ) ) ;
#2795 = DIRECTION ( 'NONE',  ( -1.000000000000000000, -0.000000000000000000, -0.000000000000000000 ) ) ;
#2796 = DIRECTION ( 'NONE',  ( -0.000000000000000000, -0.000000000000000000, -1.000000000000000000 ) ) ;
#2797 = AXIS2_PLACEMENT_3D ( 'NONE', #5899, #4998, #2352 ) ;
#2798 = CARTESIAN_POINT ( 'NONE',  ( 0.000000000000000000, 0.000000000000000000, -2.968018054819144158 ) ) ;
#2799 = FACE_OUTER_BOUND ( 'NONE', #5343, .T. ) ;
#2800 = EDGE_CURVE ( 'NONE', #11420, #1911, #7728, .T. ) ;
#2801 = ORIENTED_EDGE ( 'NONE', *, *, #5075, .T. ) ;
#2802 = DIRECTION ( 'NONE',  ( -0.000000000000000000, -0.000000000000000000, -1.000000000000000000 ) ) ;
#2803 = CARTESIAN_POINT ( 'NONE',  ( -57.61887970616808730, 55.00322141028932776, 0.004312430475834024002 ) ) ;
#2804 = CARTESIAN_POINT ( 'NONE',  ( -39.18048067635331932, 54.66929070781851152, -5.000014872209115779 ) ) ;
#2805 = CARTESIAN_POINT ( 'NONE',  ( 52.99999999999999289, 55.00000000000000000, 3.000000000000002665 ) ) ;
#2806 = CARTESIAN_POINT ( 'NONE',  ( 0.000000000000000000, 110.0000000000000000, 30.57961884250791940 ) ) ;
#2807 = ORIENTED_EDGE ( 'NONE', *, *, #10917, .T. ) ;
#2808 = CARTESIAN_POINT ( 'NONE',  ( 18.81101721030213625, 65.56418867429738384, 18.32872549916029925 ) ) ;
#2809 = CARTESIAN_POINT ( 'NONE',  ( -32.98217015207742264, 50.00000000000001421, 0.6598160721750869762 ) ) ;
#2810 = CARTESIAN_POINT ( 'NONE',  ( -78.00000000000000000, 54.99999999999999289, -1.499996628082203021 ) ) ;
#2811 = CARTESIAN_POINT ( 'NONE',  ( -22.24878634527607346, 77.42810750878007298, -11.15476345160014660 ) ) ;
#2812 = CARTESIAN_POINT ( 'NONE',  ( -75.50000000204840944, 29.18810118750000981, 10.69163855873950020 ) ) ;
#2813 = VERTEX_POINT ( 'NONE', #6656 ) ;
#2814 = AXIS2_PLACEMENT_3D ( 'NONE', #7954, #972, #3730 ) ;
#2815 = CARTESIAN_POINT ( 'NONE',  ( -78.03125000204839523, 36.74823131438024859, -18.25176868561973720 ) ) ;
#2816 = ORIENTED_EDGE ( 'NONE', *, *, #6362, .T. ) ;
#2817 = CARTESIAN_POINT ( 'NONE',  ( 8.892440619315905792, 67.93243197801977828, 21.40021590834476228 ) ) ;
#2818 = CIRCLE ( 'NONE', #3578, 1.500000000000001332 ) ;
#2819 = CARTESIAN_POINT ( 'NONE',  ( -8.503152583179597102, 66.69685394566769787, -7.822304719850006194 ) ) ;
#2820 = DIRECTION ( 'NONE',  ( -1.000000000000000000, 0.000000000000000000, 0.000000000000000000 ) ) ;
#2821 = CYLINDRICAL_SURFACE ( 'NONE', #3959, 2.500000000000000000 ) ;
#2822 = DIRECTION ( 'NONE',  ( -0.000000000000000000, -0.000000000000000000, 1.000000000000000000 ) ) ;
#2823 = AXIS2_PLACEMENT_3D ( 'NONE', #2545, #6272, #7168 ) ;
#2824 = ORIENTED_EDGE ( 'NONE', *, *, #7989, .F. ) ;
#2825 = CARTESIAN_POINT ( 'NONE',  ( -71.68677369079009054, 77.11938847399009944, 12.77062708069394503 ) ) ;
#2826 = CARTESIAN_POINT ( 'NONE',  ( -71.75000000204840944, 65.69163855873948421, -25.81189881250000440 ) ) ;
#2827 = DIRECTION ( 'NONE',  ( -1.000000000000000000, -0.000000000000000000, -0.000000000000000000 ) ) ;
#2828 = CARTESIAN_POINT ( 'NONE',  ( -58.57658864237733809, 54.99919238257378851, 0.009360382064782520051 ) ) ;
#2829 = PRODUCT_CONTEXT ( 'NONE', #7011, 'mechanical' ) ;
#2830 = AXIS2_PLACEMENT_3D ( 'NONE', #3481, #8929, #11840 ) ;
#2831 = FACE_OUTER_BOUND ( 'NONE', #3262, .T. ) ;
#2832 = CARTESIAN_POINT ( 'NONE',  ( 62.44550000000000267, 55.00000000000000000, 0.000000000000000000 ) ) ;
#2833 = EDGE_LOOP ( 'NONE', ( #2544, #11590, #7513, #1642 ) ) ;
#2834 = CARTESIAN_POINT ( 'NONE',  ( 9.813847082697366275, 50.50592320711870542, 2.216018654255096809 ) ) ;
#2835 = DIRECTION ( 'NONE',  ( 0.000000000000000000, 0.000000000000000000, 1.000000000000000000 ) ) ;
#2836 = EDGE_LOOP ( 'NONE', ( #1934, #11109, #259, #8702, #10783, #6526 ) ) ;
#2837 = CARTESIAN_POINT ( 'NONE',  ( 12.14423903554155793, 49.50741477678717928, 20.43476828740966766 ) ) ;
#2838 = CARTESIAN_POINT ( 'NONE',  ( -73.15625000204838102, 80.81189881250000440, -1.580522963032174394E-15 ) ) ;
#2839 = EDGE_CURVE ( 'NONE', #11, #10526, #2084, .T. ) ;
#2840 = ORIENTED_EDGE ( 'NONE', *, *, #5067, .T. ) ;
#2841 = DIRECTION ( 'NONE',  ( 1.000000000000000000, 0.000000000000000000, 0.000000000000000000 ) ) ;
#2842 = CARTESIAN_POINT ( 'NONE',  ( -41.78535879711923684, 60.10680040617825881, -20.39053309953287751 ) ) ;
#2843 = SURFACE_STYLE_USAGE ( .BOTH. , #3739 ) ;
#2844 = CIRCLE ( 'NONE', #10491, 5.000000000000000888 ) ;
#2845 = PLANE ( 'NONE',  #6829 ) ;
#2846 = ORIENTED_EDGE ( 'NONE', *, *, #307, .T. ) ;
#2847 = CARTESIAN_POINT ( 'NONE',  ( -4.983946421173099495, 54.34173040065561366, -4.967129911086819227 ) ) ;
#2848 = CARTESIAN_POINT ( 'NONE',  ( -5.608280846031337141, 57.05942937149918492, -21.01412426850803783 ) ) ;
#2849 = VERTEX_POINT ( 'NONE', #7071 ) ;
#2850 = CARTESIAN_POINT ( 'NONE',  ( -53.26270066237940171, 73.55098385638794412, 9.912901411881726688 ) ) ;
#2851 = AXIS2_PLACEMENT_3D ( 'NONE', #3849, #10959, #1081 ) ;
#2852 = CARTESIAN_POINT ( 'NONE',  ( -46.39182477221876866, 68.38321102182860045, -16.29532114285349920 ) ) ;
#2853 = DIRECTION ( 'NONE',  ( 0.000000000000000000, 1.000000000000000000, 0.000000000000000000 ) ) ;
#2854 = FACE_OUTER_BOUND ( 'NONE', #9476, .T. ) ;
#2855 = LINE ( 'NONE', #10154, #11835 ) ;
#2856 = LINE ( 'NONE', #10155, #4222 ) ;
#2857 = ADVANCED_FACE ( 'NONE', ( #1542 ), #8738, .F. ) ;
#2858 = VERTEX_POINT ( 'NONE', #694 ) ;
#2859 = CARTESIAN_POINT ( 'NONE',  ( 6.123233995736761352E-16, -17.82799999999998875, 4.999999999999995559 ) ) ;
#2860 = CARTESIAN_POINT ( 'NONE',  ( -58.49661103985690858, 55.00163715208778825, 0.001795710856485419104 ) ) ;
#2861 = CARTESIAN_POINT ( 'NONE',  ( -35.28845012686586102, 51.69504605834636379, -3.766257009993432270 ) ) ;
#2862 = VECTOR ( 'NONE', #4716, 1000.000000000000000 ) ;
#2863 = CARTESIAN_POINT ( 'NONE',  ( 2.500000000000000000, 0.000000000000000000, -6.099999999999999645 ) ) ;
#2864 = AXIS2_PLACEMENT_3D ( 'NONE', #1601, #5268, #697 ) ;
#2865 = DIRECTION ( 'NONE',  ( 0.000000000000000000, 1.000000000000000000, 0.000000000000000000 ) ) ;
#2866 = EDGE_CURVE ( 'NONE', #3830, #1747, #8859, .T. ) ;
#2867 = CARTESIAN_POINT ( 'NONE',  ( 3.957967453204893626, 48.00580430340492200, 0.3439981469349869259 ) ) ;
#2868 = ORIENTED_EDGE ( 'NONE', *, *, #3159, .F. ) ;
#2869 = CARTESIAN_POINT ( 'NONE',  ( 6.329456780446692576, 33.97189653527247089, -0.0004287163746460355418 ) ) ;
#2870 = UNCERTAINTY_MEASURE_WITH_UNIT (LENGTH_MEASURE( 1.000000000000000082E-05 ), #9951, 'distance_accuracy_value', 'NONE');
#2871 =( REPRESENTATION_RELATIONSHIP ('NONE','NONE', #5489, #423 ) REPRESENTATION_RELATIONSHIP_WITH_TRANSFORMATION ( #9238 )SHAPE_REPRESENTATION_RELATIONSHIP( ) );
#2872 = CARTESIAN_POINT ( 'NONE',  ( 5.000000000000000888, 0.000000000000000000, -6.099999999999999645 ) ) ;
#2873 = CARTESIAN_POINT ( 'NONE',  ( 53.00000000000000000, 51.46446609406726935, 3.535533905932731091 ) ) ;
#2874 = DIRECTION ( 'NONE',  ( 0.000000000000000000, 1.000000000000000000, 0.000000000000000000 ) ) ;
#2875 = CARTESIAN_POINT ( 'NONE',  ( -13.03788829157083207, 70.42024943993379793, -19.68589793852361680 ) ) ;
#2876 = CARTESIAN_POINT ( 'NONE',  ( -77.84375000204839523, 73.25176868561975141, -18.25176868561974430 ) ) ;
#2877 = ORIENTED_EDGE ( 'NONE', *, *, #5500, .F. ) ;
#2878 = CARTESIAN_POINT ( 'NONE',  ( -78.87500000204838102, 80.81189881250001861, 10.69163855873948599 ) ) ;
#2879 = ORIENTED_EDGE ( 'NONE', *, *, #2326, .T. ) ;
#2880 = CARTESIAN_POINT ( 'NONE',  ( 20.91744440401235039, 76.33569358685066675, -13.03537739608741575 ) ) ;
#2881 = CARTESIAN_POINT ( 'NONE',  ( -78.00000000000000000, 55.00000000000000000, -21.50000000000000000 ) ) ;
#2882 = ADVANCED_FACE ( 'NONE', ( #464 ), #6173, .F. ) ;
#2883 = CARTESIAN_POINT ( 'NONE',  ( -46.20623825043654875, 67.21094750618843250, -7.039791742250042894 ) ) ;
#2884 = CARTESIAN_POINT ( 'NONE',  ( -75.50000000204840944, 44.30836144126052289, 25.81189881250000795 ) ) ;
#2885 = CARTESIAN_POINT ( 'NONE',  ( -75.00000000000000000, 65.40507752864375846, -23.51498319519345159 ) ) ;
#2886 = CIRCLE ( 'NONE', #10134, 1.500000000000001332 ) ;
#2887 = CARTESIAN_POINT ( 'NONE',  ( 36.99999999999999289, 59.99999999999998579, 0.000000000000000000 ) ) ;
#2888 = ORIENTED_EDGE ( 'NONE', *, *, #8211, .T. ) ;
#2889 = AXIS2_PLACEMENT_3D ( 'NONE', #8039, #1617, #6195 ) ;
#2890 = LINE ( 'NONE', #11013, #359 ) ;
#2891 = CARTESIAN_POINT ( 'NONE',  ( -77.46875000409679046, 44.64466094067260826, -24.99999999999998934 ) ) ;
#2892 = CARTESIAN_POINT ( 'NONE',  ( -33.76207074264209496, 50.00000000000002842, -7.785926851161516095E-15 ) ) ;
#2893 = FACE_BOUND ( 'NONE', #11128, .T. ) ;
#2894 = CARTESIAN_POINT ( 'NONE',  ( 8.166442932151195322, 48.10666307911134254, 1.369977444835037028 ) ) ;
#2895 = CONTEXT_DEPENDENT_SHAPE_REPRESENTATION ( #2871, #4626 ) ;
#2896 = CARTESIAN_POINT ( 'NONE',  ( -21.71522205163101660, 77.00056613986325260, 0.3292152594720888503 ) ) ;
#2897 = AXIS2_PLACEMENT_3D ( 'NONE', #6862, #10374, #9541 ) ;
#2898 = CARTESIAN_POINT ( 'NONE',  ( -5.000000000000000000, 1.947085426416881093, -5.900379292880307602 ) ) ;
#2899 = EDGE_LOOP ( 'NONE', ( #2307, #2246, #10517, #5763 ) ) ;
#2900 = DIRECTION ( 'NONE',  ( 1.000000000000000000, -0.000000000000000000, 0.000000000000000000 ) ) ;
#2901 = DIRECTION ( 'NONE',  ( -1.000000000000000000, -0.000000000000000000, -0.000000000000000000 ) ) ;
#2902 = ORIENTED_EDGE ( 'NONE', *, *, #8266, .T. ) ;
#2903 = CARTESIAN_POINT ( 'NONE',  ( -20.45202553191040806, 65.80759480864719535, 18.03021102644938267 ) ) ;
#2904 = CARTESIAN_POINT ( 'NONE',  ( -76.53125000204839523, 36.74823131438024859, -18.25176868561973720 ) ) ;
#2905 = VECTOR ( 'NONE', #8919, 1000.000000000000000 ) ;
#2906 = PRODUCT_DEFINITION_SHAPE ( 'NONE', 'NONE',  #11858 ) ;
#2907 = DIRECTION ( 'NONE',  ( -1.000000000000000000, -0.000000000000000000, -0.000000000000000000 ) ) ;
#2908 = CARTESIAN_POINT ( 'NONE',  ( -19.32947785509334082, 63.04547287423799418, 19.42212676744230393 ) ) ;
#2909 = FILL_AREA_STYLE_COLOUR ( '', #1043 ) ;
#2910 = B_SPLINE_CURVE_WITH_KNOTS ( 'NONE', 1,
 ( #9446, #4001 ),
 .UNSPECIFIED., .F., .F.,
 ( 2, 2 ),
 ( 0.000000000000000000, 1.000000000000000000 ),
 .UNSPECIFIED. ) ;
#2911 = CARTESIAN_POINT ( 'NONE',  ( -59.59556320886013481, 52.94111634316250559, 20.93276532467568174 ) ) ;
#2912 = VERTEX_POINT ( 'NONE', #5090 ) ;
#2913 = CARTESIAN_POINT ( 'NONE',  ( -73.15625000204839523, 73.25176868561975141, -18.25176868561974430 ) ) ;
#2914 = CARTESIAN_POINT ( 'NONE',  ( -0.7106829068669191507, 51.23386462371114902, -3.305037806040365123 ) ) ;
#2915 = CARTESIAN_POINT ( 'NONE',  ( -79.53125000204838102, 55.00000000000000000, -25.81189881249999729 ) ) ;
#2916 = EDGE_LOOP ( 'NONE', ( #7440, #8269 ) ) ;
#2917 = CARTESIAN_POINT ( 'NONE',  ( -20.30269393938554501, 62.08599396958958039, 19.80292882502584817 ) ) ;
#2918 = CARTESIAN_POINT ( 'NONE',  ( -62.73530513678402087, 48.89572068339310107, 20.11073150603193938 ) ) ;
#2919 = LINE ( 'NONE', #4109, #5655 ) ;
#2920 = CARTESIAN_POINT ( 'NONE',  ( 24.99999999999999645, 76.00000000000000000, 0.000000000000000000 ) ) ;
#2921 = LINE ( 'NONE', #5124, #6731 ) ;
#2922 = EDGE_CURVE ( 'NONE', #3229, #8790, #11582, .T. ) ;
#2923 = ORIENTED_EDGE ( 'NONE', *, *, #6293, .T. ) ;
#2924 = CARTESIAN_POINT ( 'NONE',  ( -76.15624999999998579, 44.64466094067262958, 25.00000000000001066 ) ) ;
#2925 = CARTESIAN_POINT ( 'NONE',  ( -29.90292779502757270, 54.99043558275273114, 0.007803298580286864745 ) ) ;
#2926 = CARTESIAN_POINT ( 'NONE',  ( -38.79059579792235013, 54.34011855466147978, -4.966942020943686309 ) ) ;
#2927 = DIRECTION ( 'NONE',  ( 0.000000000000000000, 0.000000000000000000, 1.000000000000000000 ) ) ;
#2928 = DIRECTION ( 'NONE',  ( 0.000000000000000000, 0.000000000000000000, -1.000000000000000000 ) ) ;
#2929 = CARTESIAN_POINT ( 'NONE',  ( 5.417510076880946990, 48.25790868973780334, 2.048730295261496082 ) ) ;
#2930 = ORIENTED_EDGE ( 'NONE', *, *, #2555, .T. ) ;
#2931 = CARTESIAN_POINT ( 'NONE',  ( -80.00000000000001421, 67.72792206135787296, 4.242644059037073312 ) ) ;
#2932 = DIRECTION ( 'NONE',  ( -1.000000000000000000, -0.000000000000000000, -0.000000000000000000 ) ) ;
#2933 = CARTESIAN_POINT ( 'NONE',  ( -78.00000000000002842, 46.51471862576140381, 3.371917798797308130E-06 ) ) ;
#2934 = CARTESIAN_POINT ( 'NONE',  ( -2.500000000000003553, 4.330127018922192761, 0.000000000000000000 ) ) ;
#2935 = CARTESIAN_POINT ( 'NONE',  ( -16.15483550849972261, 72.60971644880963538, -17.79106955704961024 ) ) ;
#2936 = CARTESIAN_POINT ( 'NONE',  ( -73.90625000204838102, 29.18810118750000271, 4.741568889096522788E-15 ) ) ;
#2937 = EDGE_CURVE ( 'NONE', #4386, #932, #7392, .T. ) ;
#2938 = ORIENTED_EDGE ( 'NONE', *, *, #6952, .T. ) ;
#2939 = EDGE_CURVE ( 'NONE', #9073, #10129, #1597, .T. ) ;
#2940 = ADVANCED_FACE ( 'NONE', ( #3398 ), #6054, .F. ) ;
#2941 = CARTESIAN_POINT ( 'NONE',  ( -75.87500000409677625, 55.00000000000000000, -24.99999999999999645 ) ) ;
#2942 = ORIENTED_EDGE ( 'NONE', *, *, #11763, .T. ) ;
#2943 = CARTESIAN_POINT ( 'NONE',  ( -64.12603728547384208, 43.79068664598788274, 8.623361052036228713 ) ) ;
#2944 = LINE ( 'NONE', #5644, #2121 ) ;
#2945 = CARTESIAN_POINT ( 'NONE',  ( -75.00000000000001421, 58.46699551781524917, -25.57799957749213604 ) ) ;
#2946 = EDGE_CURVE ( 'NONE', #9538, #5122, #7903, .T. ) ;
#2947 = EDGE_CURVE ( 'NONE', #5798, #1761, #8151, .T. ) ;
#2948 = DIRECTION ( 'NONE',  ( 0.000000000000000000, 0.000000000000000000, 1.000000000000000000 ) ) ;
#2949 = ORIENTED_EDGE ( 'NONE', *, *, #9448, .T. ) ;
#2950 = EDGE_CURVE ( 'NONE', #1664, #6890, #3941, .T. ) ;
#2951 = DIRECTION ( 'NONE',  ( 0.000000000000000000, 0.000000000000000000, 1.000000000000000000 ) ) ;
#2952 = CARTESIAN_POINT ( 'NONE',  ( -36.48177824941181058, 50.50603341324405449, -2.216217228574558273 ) ) ;
#2953 = VECTOR ( 'NONE', #10579, 1000.000000000000000 ) ;
#2954 = CYLINDRICAL_SURFACE ( 'NONE', #938, 1.500000000000000444 ) ;
#2955 = CARTESIAN_POINT ( 'NONE',  ( 22.55679944818120575, 61.13996205570565934, 3.535017745053270044 ) ) ;
#2956 = CARTESIAN_POINT ( 'NONE',  ( -10.66763792956113832, 68.68038312560416614, 17.25573023236997372 ) ) ;
#2957 = DIRECTION ( 'NONE',  ( -1.000000000000000000, -0.000000000000000000, -0.000000000000000000 ) ) ;
#2958 = ORIENTED_EDGE ( 'NONE', *, *, #4675, .T. ) ;
#2959 = DIRECTION ( 'NONE',  ( 1.000000000000000000, 6.033820786006286457E-17, -0.000000000000000000 ) ) ;
#2960 = CARTESIAN_POINT ( 'NONE',  ( -78.00000000000002842, 46.51471862576140381, 8.485284746156354529 ) ) ;
#2961 = EDGE_LOOP ( 'NONE', ( #2064, #2433, #6422, #10980 ) ) ;
#2962 = CARTESIAN_POINT ( 'NONE',  ( -10.83980928483403794, 72.54296691076741865, -11.73126556815853760 ) ) ;
#2963 = CARTESIAN_POINT ( 'NONE',  ( -77.65625000204839523, 73.25176868561975141, -18.25176868561974430 ) ) ;
#2964 = CARTESIAN_POINT ( 'NONE',  ( -80.00000000000002842, 54.99999999999998579, 16.97056612039490986 ) ) ;
#2965 = CARTESIAN_POINT ( 'NONE',  ( -65.17448922114576249, 36.67438677247554324, 10.54995967583099237 ) ) ;
#2966 = LINE ( 'NONE', #10438, #1641 ) ;
#2967 = ORIENTED_EDGE ( 'NONE', *, *, #8112, .F. ) ;
#2968 = DIRECTION ( 'NONE',  ( 0.000000000000000000, 1.000000000000000000, 0.000000000000000000 ) ) ;
#2969 = FACE_OUTER_BOUND ( 'NONE', #2000, .T. ) ;
#2970 = CARTESIAN_POINT ( 'NONE',  ( 16.81101720596863203, 65.56606704192360269, 18.33326034385300574 ) ) ;
#2971 = COLOUR_RGB ( '',0.8941176470588234615, 0.8941176470588234615, 0.8941176470588234615 ) ;
#2972 = EDGE_LOOP ( 'NONE', ( #11157, #1177, #234, #3771 ) ) ;
#2973 = CARTESIAN_POINT ( 'NONE',  ( -19.99614452984508262, 63.04554348432252198, 19.42230297928623628 ) ) ;
#2974 = CARTESIAN_POINT ( 'NONE',  ( 4.296995438882074581, 41.00607614374722942, 0.6876389650848340196 ) ) ;
#2975 = CARTESIAN_POINT ( 'NONE',  ( -73.43750000409677625, 37.32233047033631124, 17.67766952966369232 ) ) ;
#2976 = DIRECTION ( 'NONE',  ( -6.033820786006286457E-17, 1.000000000000000000, 0.000000000000000000 ) ) ;
#2977 = CARTESIAN_POINT ( 'NONE',  ( -80.00000000000001421, 67.72792206135787296, -2.742637315201482462 ) ) ;
#2978 = DIRECTION ( 'NONE',  ( 1.000000000000000000, 0.000000000000000000, 0.000000000000000000 ) ) ;
#2979 = ORIENTED_EDGE ( 'NONE', *, *, #2326, .F. ) ;
#2980 = EDGE_CURVE ( 'NONE', #7344, #9472, #3338, .T. ) ;
#2981 = CARTESIAN_POINT ( 'NONE',  ( -75.31250000000000000, 72.67766952966368876, -17.67766952966368876 ) ) ;
#2982 = CARTESIAN_POINT ( 'NONE',  ( -75.00000000000000000, 54.23434559064500604, -25.81430454511032835 ) ) ;
#2983 = CARTESIAN_POINT ( 'NONE',  ( -78.50000000000000000, 55.00000000000000000, -24.99999999999999645 ) ) ;
#2984 = DIRECTION ( 'NONE',  ( -0.000000000000000000, 1.000000000000000000, 0.000000000000000000 ) ) ;
#2985 = VECTOR ( 'NONE', #10623, 1000.000000000000000 ) ;
#2986 = CARTESIAN_POINT ( 'NONE',  ( -74.93750000409677625, 37.32233047033631124, 17.67766952966369232 ) ) ;
#2987 = CARTESIAN_POINT ( 'NONE',  ( 21.55487747176179170, 62.01724152347335917, 0.9185355870624294372 ) ) ;
#2988 = ORIENTED_EDGE ( 'NONE', *, *, #3901, .T. ) ;
#2989 = DIRECTION ( 'NONE',  ( 0.000000000000000000, 1.000000000000000000, 0.000000000000000000 ) ) ;
#2990 = DIRECTION ( 'NONE',  ( 0.000000000000000000, 0.000000000000000000, -1.000000000000000000 ) ) ;
#2991 = DIRECTION ( 'NONE',  ( -1.000000000000000000, -6.033820786006286457E-17, -0.000000000000000000 ) ) ;
#2992 = CARTESIAN_POINT ( 'NONE',  ( -78.00000000000002842, 42.27207793864211283, 4.242644059037075976 ) ) ;
#2993 = CARTESIAN_POINT ( 'NONE',  ( -72.50000000204839523, 29.18810118750000981, 10.69163855873950020 ) ) ;
#2994 = CARTESIAN_POINT ( 'NONE',  ( -78.87500000204838102, 80.81189881250001861, 10.69163855873948599 ) ) ;
#2995 = AXIS2_PLACEMENT_3D ( 'NONE', #9842, #6091, #3374 ) ;
#2996 = ORIENTED_EDGE ( 'NONE', *, *, #4979, .T. ) ;
#2997 = CARTESIAN_POINT ( 'NONE',  ( -72.59375000204838102, 55.00000000000000000, 25.81189881249999729 ) ) ;
#2998 = EDGE_LOOP ( 'NONE', ( #8210, #9411, #7687, #773 ) ) ;
#2999 = CARTESIAN_POINT ( 'NONE',  ( 6.621374545548222024, 66.85921098149330533, -22.01171010686805118 ) ) ;
#3000 = CARTESIAN_POINT ( 'NONE',  ( -38.26205205313807056, 50.90420908871833205, -13.47689883053113213 ) ) ;
#3001 = COLOUR_RGB ( '',0.8941176470588234615, 0.8941176470588234615, 0.8941176470588234615 ) ;
#3002 = DIRECTION ( 'NONE',  ( 0.000000000000000000, 0.000000000000000000, 1.000000000000000000 ) ) ;
#3003 = CARTESIAN_POINT ( 'NONE',  ( 0.000000000000000000, 110.0000000000000000, 0.000000000000000000 ) ) ;
#3004 = DIRECTION ( 'NONE',  ( 0.000000000000000000, 0.000000000000000000, 1.000000000000000000 ) ) ;
#3005 = ORIENTED_EDGE ( 'NONE', *, *, #1557, .F. ) ;
#3006 = AXIS2_PLACEMENT_3D ( 'NONE', #94, #2079, #2017 ) ;
#3007 = CARTESIAN_POINT ( 'NONE',  ( -74.18750000000007105, 37.32233047033641071, -17.67766952966358573 ) ) ;
#3008 = CARTESIAN_POINT ( 'NONE',  ( -80.00000000000001421, 46.51471862576140381, -6.985278002320760571 ) ) ;
#3009 = DIRECTION ( 'NONE',  ( 0.000000000000000000, 0.000000000000000000, 1.000000000000000000 ) ) ;
#3010 = ADVANCED_FACE ( 'NONE', ( #10697 ), #4999, .T. ) ;
#3011 = CARTESIAN_POINT ( 'NONE',  ( -22.55675198223577027, 53.17748975554098934, 6.794389702512826368 ) ) ;
#3012 = CARTESIAN_POINT ( 'NONE',  ( -1.460760789256572600, 65.05635129456224774, 19.56749383220758887 ) ) ;
#3013 = AXIS2_PLACEMENT_3D ( 'NONE', #4907, #8732, #7724 ) ;
#3014 = CARTESIAN_POINT ( 'NONE',  ( -80.00000000000001421, 42.27207793864211283, -11.22791868944003824 ) ) ;
#3015 =( GEOMETRIC_REPRESENTATION_CONTEXT ( 3 ) GLOBAL_UNCERTAINTY_ASSIGNED_CONTEXT ( ( #11693 ) ) GLOBAL_UNIT_ASSIGNED_CONTEXT ( ( #10298, #4737, #9225 ) ) REPRESENTATION_CONTEXT ( 'NONE', 'WORKASPACE' ) );
#3016 = ORIENTED_EDGE ( 'NONE', *, *, #5885, .T. ) ;
#3017 = FACE_OUTER_BOUND ( 'NONE', #9790, .T. ) ;
#3018 = CARTESIAN_POINT ( 'NONE',  ( -78.00000000000001421, 59.24264068711927678, -4.242637315201482906 ) ) ;
#3019 = EDGE_CURVE ( 'NONE', #6717, #5255, #2317, .T. ) ;
#3020 = ORIENTED_EDGE ( 'NONE', *, *, #1903, .F. ) ;
#3021 = CARTESIAN_POINT ( 'NONE',  ( -27.52231952827322559, 42.10572610250680015, 16.77759997522909785 ) ) ;
#3022 = CARTESIAN_POINT ( 'NONE',  ( -71.84375000204838102, 55.00000000000000000, -25.81189881249999729 ) ) ;
#3023 = CIRCLE ( 'NONE', #1097, 1.500000000000001332 ) ;
#3024 = CARTESIAN_POINT ( 'NONE',  ( 47.00000000000000000, 2.835895769422954721E-15, 0.000000000000000000 ) ) ;
#3025 = CARTESIAN_POINT ( 'NONE',  ( -79.81250000000004263, 72.67766952966367455, -17.67766952966367100 ) ) ;
#3026 = SHAPE_REPRESENTATION_RELATIONSHIP ( 'NONE' , 'NONE' ,  #2176, #9416 ) ;
#3027 = CARTESIAN_POINT ( 'NONE',  ( -78.00000000000001421, 54.99999999999999289, -18.47055937655931501 ) ) ;
#3028 = VERTEX_POINT ( 'NONE', #6648 ) ;
#3029 = CARTESIAN_POINT ( 'NONE',  ( -73.62500000204840944, 29.18810118750000626, -10.69163855873949132 ) ) ;
#3030 = DIRECTION ( 'NONE',  ( 0.000000000000000000, 0.000000000000000000, -1.000000000000000000 ) ) ;
#3031 = CARTESIAN_POINT ( 'NONE',  ( 2.595920079249742329, 34.88763922991881827, -6.102757042485290384 ) ) ;
#3032 = ORIENTED_EDGE ( 'NONE', *, *, #5297, .T. ) ;
#3033 = CARTESIAN_POINT ( 'NONE',  ( -6.670543235071888510, 63.04736075021470754, -19.42691569015581976 ) ) ;
#3034 = CARTESIAN_POINT ( 'NONE',  ( 2.256059437406555457, 41.59371342422682716, -4.067545439913939020 ) ) ;
#3035 = CARTESIAN_POINT ( 'NONE',  ( -78.00000000000001421, 67.72792206135787296, 5.742644059037073312 ) ) ;
#3036 = CARTESIAN_POINT ( 'NONE',  ( -77.56250000409679046, 37.32233047033631124, -17.67766952966368166 ) ) ;
#3037 = CARTESIAN_POINT ( 'NONE',  ( -2.500000000000000000, 3.061616997868383141E-16, -2.103846626247716234 ) ) ;
#3038 = CARTESIAN_POINT ( 'NONE',  ( -75.49999999999972999, 55.00000000002793854, -24.99999999999999645 ) ) ;
#3039 = ORIENTED_EDGE ( 'NONE', *, *, #4619, .F. ) ;
#3040 = ADVANCED_FACE ( 'NONE', ( #5867 ), #5992, .F. ) ;
#3041 = CARTESIAN_POINT ( 'NONE',  ( -77.75000000000000000, 55.00000000000000000, 24.99999999999999645 ) ) ;
#3042 = DIRECTION ( 'NONE',  ( -0.000000000000000000, -0.000000000000000000, -1.000000000000000000 ) ) ;
#3043 = DIRECTION ( 'NONE',  ( -1.000000000000000000, -0.000000000000000000, -0.000000000000000000 ) ) ;
#3044 = AXIS2_PLACEMENT_3D ( 'NONE', #11362, #4915, #5939 ) ;
#3045 = DIRECTION ( 'NONE',  ( 0.000000000000000000, 0.000000000000000000, 1.000000000000000000 ) ) ;
#3046 = CARTESIAN_POINT ( 'NONE',  ( -63.07624402531011754, 50.93185762523746973, 13.40497886217843160 ) ) ;
#3047 = VERTEX_POINT ( 'NONE', #7602 ) ;
#3048 = CARTESIAN_POINT ( 'NONE',  ( -6.785358873008338954, 67.52118754941005818, -16.88410835930674381 ) ) ;
#3049 = CARTESIAN_POINT ( 'NONE',  ( -78.00000000000001421, 63.48528137423857487, 8.485284746156350977 ) ) ;
#3050 = B_SPLINE_CURVE_WITH_KNOTS ( 'NONE', 3,
 ( #9374, #8542, #11038, #5674, #2790, #8487, #2970, #325, #1044, #11221, #3990, #7650, #5738, #4709, #7479, #6700, #4768, #142, #3808, #8301, #1166, #9315, #3031, #10331, #6454, #1882, #9196, #987, #11100, #82, #3744, #2848, #6517, #6580, #2003, #10615, #11341, #8609, #387, #4285, #4104, #11283, #3096, #3149, #2425, #4953, #6936, #6762, #4163, #1352, #10389, #3265, #4055, #2365, #7711, #5132, #2245, #8666, #6037, #7762, #2185, #6817, #5190, #7887, #5983, #2306, #8842, #5018, #1526, #8718, #10442, #446, #5855, #9558, #11393, #1469, #5914, #3206, #6875, #561, #501, #621, #1412, #9672, #10502, #6094, #9496, #9617, #5074, #1286, #7823, #11456, #8780, #10564, #4228, #11518, #3324, #6992, #9726, #677, #5365, #4350, #9017, #5250, #6274, #11577, #7942, #9789, #4467, #6153, #6332, #8897, #5422, #9961, #9072, #848, #10916, #3379, #7232, #4519, #7170, #793, #1809, #10739 ),
 .UNSPECIFIED., .F., .F.,
 ( 4, 2, 2, 2, 2, 2, 2, 2, 2, 2, 2, 2, 2, 2, 2, 2, 2, 2, 2, 2, 2, 2, 2, 2, 2, 2, 2, 2, 2, 2, 2, 2, 2, 2, 2, 2, 2, 2, 2, 2, 2, 2, 2, 2, 2, 2, 2, 2, 2, 2, 2, 2, 2, 2, 2, 2, 2, 2, 2, 2, 2, 4 ),
 ( 0.000000000000000000, 0.02499977550252127645, 0.04999988577693819519, 0.07499999605135511394, 0.09999999831535408279, 0.1250000005793530378, 0.1500000028441162425, 0.1750000051088794195, 0.1937500039558066045, 0.2031250033792701970, 0.2125000028027338173, 0.2218750022261974375, 0.2312500016496610300, 0.2500000004965882150, 0.2750000027613288545, 0.3000000050260694384, 0.3187500038730080032, 0.3281250032964772578, 0.3375000027199465125, 0.3468750021434158226, 0.3562500015668850772, 0.3750000004138236420, 0.4000000026785641705, 0.4250000049433046989, 0.4437500037902432082, 0.4531250032137125183, 0.4625000026371817730, 0.4718750020606510276, 0.4812500014841203377, 0.5000000003310588470, 0.5250000025957997085, 0.5500000048605405700, 0.5687500037074788573, 0.5781250031309480564, 0.5875000025544172555, 0.5968750019778864546, 0.6062500014013556537, 0.6250000002482940520, 0.6500000025128280789, 0.6750000047773621059, 0.6937500036244039769, 0.7031250030479249125, 0.7125000024714458480, 0.7218750018949667835, 0.7312500013184877190, 0.7500000001655295900, 0.7750000023794885173, 0.8000000045934475557, 0.8187500034657768655, 0.8281250029019414649, 0.8375000023381060643, 0.8468750017742707747, 0.8562500012104353742, 0.8750000000827646840, 0.8937502654913498379, 0.9031253981956424148, 0.9125005308999349918, 0.9218756636042275687, 0.9312507963085201457, 0.9500010617171052996, 0.9750005308585526498, 1.000000000000000000 ),
 .UNSPECIFIED. ) ;
#3051 = DIRECTION ( 'NONE',  ( 0.000000000000000000, 0.000000000000000000, 1.000000000000000000 ) ) ;
#3052 = DIRECTION ( 'NONE',  ( -0.8191520442889974607, 0.000000000000000000, -0.5735764363510379438 ) ) ;
#3053 = CARTESIAN_POINT ( 'NONE',  ( -25.03835002304701973, 79.78434740670915915, 3.387367328291911672 ) ) ;
#3054 = CARTESIAN_POINT ( 'NONE',  ( -78.12500000204838102, 29.18810118750000626, -10.69163855873949309 ) ) ;
#3055 = ORIENTED_EDGE ( 'NONE', *, *, #2693, .T. ) ;
#3056 = CARTESIAN_POINT ( 'NONE',  ( -72.03125000204839523, 36.74823131438024859, -18.25176868561973720 ) ) ;
#3057 = AXIS2_PLACEMENT_3D ( 'NONE', #4248, #6232, #6956 ) ;
#3058 = CARTESIAN_POINT ( 'NONE',  ( -75.78125000000005684, 30.00000000000011013, -10.35533905932734022 ) ) ;
#3059 = FACE_OUTER_BOUND ( 'NONE', #11831, .T. ) ;
#3060 = AXIS2_PLACEMENT_3D ( 'NONE', #10748, #6223, #7180 ) ;
#3061 = CARTESIAN_POINT ( 'NONE',  ( -28.92281818629570722, 41.57851372300513049, 4.073127600961401029 ) ) ;
#3062 = EDGE_CURVE ( 'NONE', #5122, #6726, #11232, .T. ) ;
#3063 = DIRECTION ( 'NONE',  ( 0.000000000000000000, 0.000000000000000000, 1.000000000000000000 ) ) ;
#3064 = DIRECTION ( 'NONE',  ( 0.000000000000000000, 0.000000000000000000, 1.000000000000000000 ) ) ;
#3065 = DIRECTION ( 'NONE',  ( -0.000000000000000000, -0.000000000000000000, -1.000000000000000000 ) ) ;
#3066 = CIRCLE ( 'NONE', #10119, 9.999999999999987566 ) ;
#3067 = EDGE_LOOP ( 'NONE', ( #10211, #5606, #167, #7804 ) ) ;
#3068 = CARTESIAN_POINT ( 'NONE',  ( -75.50000000000000000, 55.00000000000000000, -24.99999999999999645 ) ) ;
#3069 = CARTESIAN_POINT ( 'NONE',  ( -72.68750000409677625, 72.67766952966368876, -17.67766952966368876 ) ) ;
#3070 = CARTESIAN_POINT ( 'NONE',  ( -49.71141041926628645, 59.49513311707226393, -2.214139657851166287 ) ) ;
#3071 = ORIENTED_EDGE ( 'NONE', *, *, #9421, .F. ) ;
#3072 = EDGE_CURVE ( 'NONE', #11556, #4778, #11195, .T. ) ;
#3073 = CARTESIAN_POINT ( 'NONE',  ( -1.556678960741344708, 54.08359337848497006, -6.974639707943993017 ) ) ;
#3074 = AXIS2_PLACEMENT_3D ( 'NONE', #2933, #881, #5636 ) ;
#3075 = CARTESIAN_POINT ( 'NONE',  ( -15.87820011566687484, 72.30454950739435560, 13.62882577052523558 ) ) ;
#3076 = DIRECTION ( 'NONE',  ( -1.000000000000000000, -0.000000000000000000, -0.000000000000000000 ) ) ;
#3077 = ORIENTED_EDGE ( 'NONE', *, *, #3309, .F. ) ;
#3078 = CARTESIAN_POINT ( 'NONE',  ( -71.38989868722833876, 76.65063840437913711, 12.49999426730988361 ) ) ;
#3079 = CARTESIAN_POINT ( 'NONE',  ( -77.65625000204838102, 80.81189881250000440, -1.580522963032174394E-15 ) ) ;
#3080 = EDGE_LOOP ( 'NONE', ( #5000, #1476 ) ) ;
#3081 = CARTESIAN_POINT ( 'NONE',  ( -43.78535878948660098, 60.10716095388539060, -20.39140800440753054 ) ) ;
#3082 = CARTESIAN_POINT ( 'NONE',  ( -72.31250000204839523, 29.18810118750000981, 10.69163855873950020 ) ) ;
#3083 = EDGE_CURVE ( 'NONE', #3150, #2603, #5811, .T. ) ;
#3084 = EDGE_CURVE ( 'NONE', #5117, #8038, #2910, .T. ) ;
#3085 = CYLINDRICAL_SURFACE ( 'NONE', #2320, 2.500000000000000000 ) ;
#3086 = CARTESIAN_POINT ( 'NONE',  ( -61.63584152524990145, 46.00569487729882212, 19.01260273971552905 ) ) ;
#3087 = VECTOR ( 'NONE', #2529, 1000.000000000000000 ) ;
#3088 = AXIS2_PLACEMENT_3D ( 'NONE', #8704, #7928, #9655 ) ;
#3089 =( NAMED_UNIT ( * ) SI_UNIT ( $, .STERADIAN. ) SOLID_ANGLE_UNIT ( ) );
#3090 = DIRECTION ( 'NONE',  ( 0.000000000000000000, 1.000000000000000000, 0.000000000000000000 ) ) ;
#3091 = ORIENTED_EDGE ( 'NONE', *, *, #10975, .F. ) ;
#3092 = CARTESIAN_POINT ( 'NONE',  ( -72.50000000204836681, 44.30836144126052289, 25.81189881250000795 ) ) ;
#3093 = CARTESIAN_POINT ( 'NONE',  ( -1.482474291011559364, 51.69668081413308158, -3.767642887559051079 ) ) ;
#3094 =( BOUNDED_CURVE ( )  B_SPLINE_CURVE ( 2, ( #2405, #6257, #6198, #4144, #544, #4208, #6020, #10660, #487 ),
 .UNSPECIFIED., .F., .T. ) 
 B_SPLINE_CURVE_WITH_KNOTS ( ( 3, 2, 2, 2, 3 ),
 ( 0.000000000000000000, 0.02083333333333334952, 0.04166666666666669905, 0.06250000000000005551, 0.08333333333333339810 ),
 .UNSPECIFIED. ) 
 CURVE ( )  GEOMETRIC_REPRESENTATION_ITEM ( )  RATIONAL_B_SPLINE_CURVE ( ( 1.000000000000000000, 0.9238795325112867385, 1.000000000000000000, 0.9238795325112867385, 1.000000000000000000, 0.9238795325112867385, 1.000000000000000000, 0.9238795325112865164, 1.000000000000000222 ) ) 
 REPRESENTATION_ITEM ( '' )  );
#3095 = EDGE_CURVE ( 'NONE', #1776, #5647, #9569, .T. ) ;
#3096 = CARTESIAN_POINT ( 'NONE',  ( -11.39182375260447166, 73.60042400440836730, -9.933379572949093017 ) ) ;
#3097 = ORIENTED_EDGE ( 'NONE', *, *, #291, .T. ) ;
#3098 = CARTESIAN_POINT ( 'NONE',  ( 4.996123431639940549, 33.97227858069939543, -0.0004331113196134536714 ) ) ;
#3099 = AXIS2_PLACEMENT_3D ( 'NONE', #10764, #9152, #5393 ) ;
#3100 = CARTESIAN_POINT ( 'NONE',  ( -56.63607177307330431, 69.12418599258134577, 15.58301102096070245 ) ) ;
#3101 = CARTESIAN_POINT ( 'NONE',  ( 19.99999999999996803, -57.00000000000000000, 5.000000000000000000 ) ) ;
#3102 = CARTESIAN_POINT ( 'NONE',  ( -78.00000000000001421, 67.72792206135787296, 12.72792543327562775 ) ) ;
#3103 = EDGE_CURVE ( 'NONE', #2643, #9669, #10453, .T. ) ;
#3104 = CARTESIAN_POINT ( 'NONE',  ( 53.00000000000000000, 51.46446609406726935, -3.535533905932738197 ) ) ;
#3105 = ORIENTED_EDGE ( 'NONE', *, *, #6552, .F. ) ;
#3106 = CARTESIAN_POINT ( 'NONE',  ( -77.00000000000000000, 55.00000000000000000, -24.99999999999999645 ) ) ;
#3107 = CARTESIAN_POINT ( 'NONE',  ( 39.99999999999999289, 55.00000000000000000, 24.99999999999999645 ) ) ;
#3108 =( LENGTH_UNIT ( ) NAMED_UNIT ( * ) SI_UNIT ( .MILLI., .METRE. ) );
#3109 = DIRECTION ( 'NONE',  ( 0.000000000000000000, 1.000000000000000000, 0.000000000000000000 ) ) ;
#3110 = CARTESIAN_POINT ( 'NONE',  ( 12.22341952602966764, 54.08367749976515171, 7.017190178460947614 ) ) ;
#3111 = ORIENTED_EDGE ( 'NONE', *, *, #6989, .F. ) ;
#3112 = CARTESIAN_POINT ( 'NONE',  ( -37.18898618307433424, 44.43582214169357769, -18.32873044267784479 ) ) ;
#3113 = DIRECTION ( 'NONE',  ( 1.000000000000000000, 0.000000000000000000, 0.000000000000000000 ) ) ;
#3114 = DIRECTION ( 'NONE',  ( -1.000000000000000000, 0.000000000000000000, 0.000000000000000000 ) ) ;
#3115 = CARTESIAN_POINT ( 'NONE',  ( -79.15625000204839523, 73.25176868561975141, -18.25176868561974430 ) ) ;
#3116 = FACE_BOUND ( 'NONE', #7219, .T. ) ;
#3117 = CARTESIAN_POINT ( 'NONE',  ( -74.28125000204838102, 55.00000000000000000, 25.81189881249999729 ) ) ;
#3118 = EDGE_LOOP ( 'NONE', ( #11704, #1583, #3135, #3342 ) ) ;
#3119 = CARTESIAN_POINT ( 'NONE',  ( -77.00000000409677625, 80.00000000000000000, -1.530808498934191324E-15 ) ) ;
#3120 = ORIENTED_EDGE ( 'NONE', *, *, #5936, .F. ) ;
#3121 = CARTESIAN_POINT ( 'NONE',  ( 24.87203822307476031, 79.64205355216036253, 4.236592033986310568 ) ) ;
#3122 = CARTESIAN_POINT ( 'NONE',  ( -60.12103580250087731, 51.59597441208588720, 13.59059695706972626 ) ) ;
#3123 = CARTESIAN_POINT ( 'NONE',  ( -78.40625000204838102, 29.18810118750000271, 4.741568889096522788E-15 ) ) ;
#3124 = CARTESIAN_POINT ( 'NONE',  ( -75.00000000000001421, 77.22263599570800352, 11.53795789873604427 ) ) ;
#3125 = CARTESIAN_POINT ( 'NONE',  ( -73.34375000000007105, 65.35533905932732068, 24.99999999999986500 ) ) ;
#3126 = ORIENTED_EDGE ( 'NONE', *, *, #9968, .F. ) ;
#3127 = CARTESIAN_POINT ( 'NONE',  ( -76.34375000000001421, 65.35533905932737753, 24.99999999999999645 ) ) ;
#3128 = CARTESIAN_POINT ( 'NONE',  ( -73.43750000409677625, 37.32233047033631124, 17.67766952966369232 ) ) ;
#3129 = FACE_OUTER_BOUND ( 'NONE', #8174, .T. ) ;
#3130 = ORIENTED_EDGE ( 'NONE', *, *, #799, .T. ) ;
#3131 = EDGE_CURVE ( 'NONE', #9206, #6608, #7661, .T. ) ;
#3132 = CARTESIAN_POINT ( 'NONE',  ( -16.91627854707998679, 59.45272466182848348, 5.424304687769180511 ) ) ;
#3133 = CARTESIAN_POINT ( 'NONE',  ( -9.505256967967094184, 67.97321577359559797, 17.78506628848226256 ) ) ;
#3134 = DIRECTION ( 'NONE',  ( 0.000000000000000000, 0.000000000000000000, 1.000000000000000000 ) ) ;
#3135 = ORIENTED_EDGE ( 'NONE', *, *, #1110, .T. ) ;
#3136 = DIRECTION ( 'NONE',  ( 0.000000000000000000, 1.000000000000000000, 0.000000000000000000 ) ) ;
#3137 = CARTESIAN_POINT ( 'NONE',  ( -75.78125000204838102, 55.00000000000000000, 25.81189881249999729 ) ) ;
#3138 = ORIENTED_EDGE ( 'NONE', *, *, #7338, .T. ) ;
#3139 = CARTESIAN_POINT ( 'NONE',  ( -23.05849041873830885, 57.05917197429855037, 20.98589082339331569 ) ) ;
#3140 = AXIS2_PLACEMENT_3D ( 'NONE', #7132, #2563, #3517 ) ;
#3141 = LINE ( 'NONE', #2056, #6714 ) ;
#3142 = DIRECTION ( 'NONE',  ( -0.000000000000000000, 0.000000000000000000, -1.000000000000000000 ) ) ;
#3143 = CARTESIAN_POINT ( 'NONE',  ( -60.73530621856283318, 48.89645762657089278, 20.10868697360108115 ) ) ;
#3144 = DIRECTION ( 'NONE',  ( -0.000000000000000000, -0.000000000000000000, -1.000000000000000000 ) ) ;
#3145 = ORIENTED_EDGE ( 'NONE', *, *, #3317, .T. ) ;
#3146 = FACE_OUTER_BOUND ( 'NONE', #15, .T. ) ;
#3147 = FACE_OUTER_BOUND ( 'NONE', #6044, .T. ) ;
#3148 = PRODUCT_DEFINITION ( 'UNKNOWN', '', #6047, #11555 ) ;
#3149 = CARTESIAN_POINT ( 'NONE',  ( -12.81092923270300865, 75.46953867936616689, -5.507006106411301616 ) ) ;
#3150 = VERTEX_POINT ( 'NONE', #10342 ) ;
#3151 = CARTESIAN_POINT ( 'NONE',  ( -69.00771387827577996, 33.99486225849476995, 0.006699851613120169809 ) ) ;
#3152 = CARTESIAN_POINT ( 'NONE',  ( -34.50315233865081410, 41.19915729885462952, -2.739730459386737316 ) ) ;
#3153 = DIRECTION ( 'NONE',  ( -1.000000000000000000, -0.000000000000000000, -0.000000000000000000 ) ) ;
#3154 = CARTESIAN_POINT ( 'NONE',  ( -77.46875000409679046, 44.64466094067266511, -25.00000000000004263 ) ) ;
#3155 = DIRECTION ( 'NONE',  ( 1.000000000000000000, 0.000000000000000000, 0.000000000000000000 ) ) ;
#3156 = ORIENTED_EDGE ( 'NONE', *, *, #3084, .T. ) ;
#3157 = CARTESIAN_POINT ( 'NONE',  ( -78.12500000000000000, 80.00000000000000000, -1.530808498934191324E-15 ) ) ;
#3158 = CARTESIAN_POINT ( 'NONE',  ( -61.99733827119050744, 54.99927236536940711, 0.002460332904419732219 ) ) ;
#3159 = EDGE_CURVE ( 'NONE', #2858, #131, #1340, .T. ) ;
#3160 = PRODUCT_DEFINITION_FORMATION_WITH_SPECIFIED_SOURCE ( 'ANY', '', #10530, .NOT_KNOWN. ) ;
#3161 = CARTESIAN_POINT ( 'NONE',  ( -78.00000000000001421, 67.72792206135787296, -14.22791868944004356 ) ) ;
#3162 = PLANE ( 'NONE',  #10650 ) ;
#3163 = CARTESIAN_POINT ( 'NONE',  ( -14.22341865602713007, 61.98282206426377883, -0.9163204132140592151 ) ) ;
#3164 = ORIENTED_EDGE ( 'NONE', *, *, #1682, .F. ) ;
#3165 = CARTESIAN_POINT ( 'NONE',  ( -50.82691677660828589, 75.68920158268997511, 4.121780573430135597 ) ) ;
#3166 = EDGE_CURVE ( 'NONE', #8985, #6801, #11294, .T. ) ;
#3167 = CARTESIAN_POINT ( 'NONE',  ( -78.00000000000001421, 67.72792206135787296, 12.72792543327562775 ) ) ;
#3168 = CARTESIAN_POINT ( 'NONE',  ( 0.000000000000000000, 0.000000000000000000, -0.01270000000000047133 ) ) ;
#3169 = EDGE_CURVE ( 'NONE', #11498, #10642, #3509, .T. ) ;
#3170 = CARTESIAN_POINT ( 'NONE',  ( -74.65625000204839523, 73.25176868561975141, -18.25176868561974430 ) ) ;
#3171 = CARTESIAN_POINT ( 'NONE',  ( -75.96875000000005684, 30.00000000000011013, 10.35533905932735088 ) ) ;
#3172 = CARTESIAN_POINT ( 'NONE',  ( -77.46875000204839523, 80.81189881250000440, -1.580522963032174394E-15 ) ) ;
#3173 = ORIENTED_EDGE ( 'NONE', *, *, #2725, .F. ) ;
#3174 = CARTESIAN_POINT ( 'NONE',  ( -78.78125000409679046, 65.35533905932737753, -24.99999999999999645 ) ) ;
#3175 = LINE ( 'NONE', #11082, #11641 ) ;
#3176 = ORIENTED_EDGE ( 'NONE', *, *, #6074, .T. ) ;
#3177 = CARTESIAN_POINT ( 'NONE',  ( -25.52231952398968673, 42.10919693116569817, 16.77412918608628090 ) ) ;
#3178 = CARTESIAN_POINT ( 'NONE',  ( -75.00000000000001421, 58.46699551781524917, -25.57799957749213604 ) ) ;
#3179 = CARTESIAN_POINT ( 'NONE',  ( 34.00000000000000000, 59.99999999999998579, 0.000000000000000000 ) ) ;
#3180 = DIRECTION ( 'NONE',  ( -1.000000000000000000, 0.000000000000000000, -0.000000000000000000 ) ) ;
#3181 = ORIENTED_EDGE ( 'NONE', *, *, #10879, .F. ) ;
#3182 = CARTESIAN_POINT ( 'NONE',  ( 2.500000000000003109, -4.330127018922193649, -6.099999999999999645 ) ) ;
#3183 = CARTESIAN_POINT ( 'NONE',  ( -75.87500000000000000, 30.00000000000000355, 4.592425496802573578E-15 ) ) ;
#3184 = CARTESIAN_POINT ( 'NONE',  ( -73.62500000409677625, 55.00000000000000000, 24.99999999999999645 ) ) ;
#3185 = CARTESIAN_POINT ( 'NONE',  ( 0.000000000000000000, 0.000000000000000000, -0.8895714285714284575 ) ) ;
#3186 = ORIENTED_EDGE ( 'NONE', *, *, #2555, .F. ) ;
#3187 = EDGE_CURVE ( 'NONE', #6484, #1706, #8968, .T. ) ;
#3188 = CARTESIAN_POINT ( 'NONE',  ( -48.22334500059429274, 61.97465389400121438, -0.9164071902225618960 ) ) ;
#3189 = CARTESIAN_POINT ( 'NONE',  ( 0.000000000000000000, 50.00000000000000000, 0.000000000000000000 ) ) ;
#3190 =( NAMED_UNIT ( * ) SI_UNIT ( $, .STERADIAN. ) SOLID_ANGLE_UNIT ( ) );
#3191 = ORIENTED_EDGE ( 'NONE', *, *, #445, .F. ) ;
#3192 = CARTESIAN_POINT ( 'NONE',  ( 9.475534631369814775, 67.98327214991455492, -17.76592228101513271 ) ) ;
#3193 = CIRCLE ( 'NONE', #3006, 4.999999999999997335 ) ;
#3194 = CARTESIAN_POINT ( 'NONE',  ( -79.15625000204838102, 80.81189881250000440, -1.580522963032174394E-15 ) ) ;
#3195 = CONICAL_SURFACE ( 'NONE', #9883, 3.000000000000000000, 0.9599310885968912466 ) ;
#3196 = EDGE_LOOP ( 'NONE', ( #7308, #9981 ) ) ;
#3197 = DIRECTION ( 'NONE',  ( -1.000000000000000000, -0.000000000000000000, -0.000000000000000000 ) ) ;
#3198 = CARTESIAN_POINT ( 'NONE',  ( 2.500000000000000000, 0.000000000000000000, -1.403639088038009630 ) ) ;
#3199 = CARTESIAN_POINT ( 'NONE',  ( -79.62500000000001421, 79.99999999999997158, -1.530808498934189944E-15 ) ) ;
#3200 = DIRECTION ( 'NONE',  ( -0.000000000000000000, -0.000000000000000000, 1.000000000000000000 ) ) ;
#3201 = EDGE_CURVE ( 'NONE', #4223, #10886, #6281, .T. ) ;
#3202 = ORIENTED_EDGE ( 'NONE', *, *, #1871, .T. ) ;
#3203 = LINE ( 'NONE', #1468, #9891 ) ;
#3204 = B_SPLINE_CURVE_WITH_KNOTS ( 'NONE', 3,
 ( #5615, #2127, #3989, #4889, #5737, #1042, #3806, #4708, #11281, #5800, #2914, #3093, #9434, #8360, #4767, #6579, #10209, #2847, #10083, #2002, #1222, #7649, #1880, #986, #1164, #9195, #4834, #8486, #7590, #4647, #8422, #8300, #80, #3743, #11559, #10441, #9772, #2470 ),
 .UNSPECIFIED., .F., .F.,
 ( 4, 2, 2, 2, 2, 2, 2, 2, 2, 2, 2, 2, 2, 2, 2, 2, 2, 2, 4 ),
 ( 0.02428446548970041724, 0.02580228911461803637, 0.02732011273953565550, 0.02807902455199446506, 0.02883793636445327463, 0.03035575998937089376, 0.03187358361428851289, 0.03339140723920613202, 0.03490923086412375115, 0.03642705448904137028, 0.03794487811395898247, 0.03946270173887660854, 0.04022161355133541810, 0.04098052536379422767, 0.04249834898871186067, 0.04401617261362950062, 0.04553399623854713363, 0.04705181986346476664, 0.04856964348838239964 ),
 .UNSPECIFIED. ) ;
#3205 = B_SPLINE_CURVE_WITH_KNOTS ( 'NONE', 3,
 ( #3978, #7635, #2052, #7464, #3859, #7522 ),
 .UNSPECIFIED., .F., .F.,
 ( 4, 2, 4 ),
 ( 0.005150343764683554260, 0.006610526168996383976, 0.008070708573309213693 ),
 .UNSPECIFIED. ) ;
#3206 = CARTESIAN_POINT ( 'NONE',  ( -38.47762819156672265, 42.07891330237754346, -16.80402559754432801 ) ) ;
#3207 = VERTEX_POINT ( 'NONE', #5199 ) ;
#3208 = EDGE_CURVE ( 'NONE', #10937, #6451, #2612, .T. ) ;
#3209 = CARTESIAN_POINT ( 'NONE',  ( -18.03064345808105173, 70.57358235614606201, 14.11515935890559881 ) ) ;
#3210 = CARTESIAN_POINT ( 'NONE',  ( -43.25615049311128502, 56.37302494055165170, -13.95606205737922423 ) ) ;
#3211 = FACE_OUTER_BOUND ( 'NONE', #5333, .T. ) ;
#3212 = DIRECTION ( 'NONE',  ( 0.000000000000000000, 1.000000000000000000, 0.000000000000000000 ) ) ;
#3213 = CARTESIAN_POINT ( 'NONE',  ( -18.20729755437997710, 59.33894261634819145, 2.506317759643504228 ) ) ;
#3214 = ORIENTED_EDGE ( 'NONE', *, *, #3934, .F. ) ;
#3215 = CARTESIAN_POINT ( 'NONE',  ( -77.56250000204838102, 80.81189881250001861, 10.69163855873948599 ) ) ;
#3216 = CARTESIAN_POINT ( 'NONE',  ( -74.99999999999998579, 46.81069822181994056, -24.49304663887657796 ) ) ;
#3217 = DIRECTION ( 'NONE',  ( 1.000000000000000000, 0.000000000000000000, 0.000000000000000000 ) ) ;
#3218 = CIRCLE ( 'NONE', #9909, 9.999999999999987566 ) ;
#3219 = DIRECTION ( 'NONE',  ( -1.000000000000000000, -0.000000000000000000, -0.000000000000000000 ) ) ;
#3220 = CARTESIAN_POINT ( 'NONE',  ( -29.58248992310308978, 49.55513497353873476, 4.472866631367526935 ) ) ;
#3221 = VERTEX_POINT ( 'NONE', #4174 ) ;
#3222 = CARTESIAN_POINT ( 'NONE',  ( -51.69727455458300369, 74.78870212167194609, 7.080596778485133136 ) ) ;
#3223 = CARTESIAN_POINT ( 'NONE',  ( 21.47754340280339136, 75.43473409906381733, 5.492671141289128478 ) ) ;
#3224 = EDGE_CURVE ( 'NONE', #678, #1342, #682, .T. ) ;
#3225 = CARTESIAN_POINT ( 'NONE',  ( -75.00000000000000000, 55.00000000000000000, 25.00000000000000355 ) ) ;
#3226 = CARTESIAN_POINT ( 'NONE',  ( -74.56250000204839523, 80.81189881250000440, -10.69163855873948954 ) ) ;
#3227 = CARTESIAN_POINT ( 'NONE',  ( -5.843944843092907071, 66.54774434410467165, 22.17515753471153772 ) ) ;
#3228 = CARTESIAN_POINT ( 'NONE',  ( -74.84375000204839523, 55.00000000000000000, -25.81189881249999729 ) ) ;
#3229 = VERTEX_POINT ( 'NONE', #3273 ) ;
#3230 = DIRECTION ( 'NONE',  ( 0.000000000000000000, 0.000000000000000000, 1.000000000000000000 ) ) ;
#3231 = CARTESIAN_POINT ( 'NONE',  ( -78.00000000000000000, 55.00000000000000000, 0.000000000000000000 ) ) ;
#3232 = ORIENTED_EDGE ( 'NONE', *, *, #5875, .T. ) ;
#3233 = CARTESIAN_POINT ( 'NONE',  ( -15.82693394478133797, 72.53700911420227726, 11.72543866452437733 ) ) ;
#3234 = CARTESIAN_POINT ( 'NONE',  ( 0.000000000000000000, 0.000000000000000000, -4.346257142857142597 ) ) ;
#3235 = VECTOR ( 'NONE', #859, 1000.000000000000000 ) ;
#3236 = CARTESIAN_POINT ( 'NONE',  ( -75.00000000000000000, 76.68791387293471473, 12.43520775219157315 ) ) ;
#3237 = DIRECTION ( 'NONE',  ( 0.8191520442889974607, 1.003171929053531649E-16, -0.5735764363510379438 ) ) ;
#3238 = ORIENTED_EDGE ( 'NONE', *, *, #9059, .F. ) ;
#3239 = DIRECTION ( 'NONE',  ( -0.000000000000000000, -0.000000000000000000, -1.000000000000000000 ) ) ;
#3240 = AXIS2_PLACEMENT_3D ( 'NONE', #7333, #8333, #8465 ) ;
#3241 = CARTESIAN_POINT ( 'NONE',  ( -75.31250000000000000, 72.67766952966368876, -17.67766952966368876 ) ) ;
#3242 = CARTESIAN_POINT ( 'NONE',  ( 4.182066831946701591, -3.358985280702831755, -0.1739375980333770777 ) ) ;
#3243 = CIRCLE ( 'NONE', #4970, 4.999999999999997335 ) ;
#3244 = ADVANCED_FACE ( 'NONE', ( #10687 ), #3557, .T. ) ;
#3245 = CARTESIAN_POINT ( 'NONE',  ( -46.20572079224533724, 57.50577717681836276, -4.339287318856722919 ) ) ;
#3246 = ORIENTED_EDGE ( 'NONE', *, *, #8926, .F. ) ;
#3247 = CARTESIAN_POINT ( 'NONE',  ( -38.50022373450124036, 53.63002255421522335, -6.893336926830083478 ) ) ;
#3248 = CARTESIAN_POINT ( 'NONE',  ( -75.00000000000000000, 55.00000000000000000, 0.000000000000000000 ) ) ;
#3249 = CARTESIAN_POINT ( 'NONE',  ( 36.99999999999999289, 50.00000000000001421, 6.123233995736750505E-16 ) ) ;
#3250 = CIRCLE ( 'NONE', #4210, 1.500000000000001332 ) ;
#3251 = ORIENTED_EDGE ( 'NONE', *, *, #4742, .F. ) ;
#3252 = CARTESIAN_POINT ( 'NONE',  ( 2.920128277213786205, 65.29083636825203030, 19.44520279024829179 ) ) ;
#3253 = CARTESIAN_POINT ( 'NONE',  ( 0.000000000000000000, 5.773502691896260863, -5.653418012614792154 ) ) ;
#3254 = ORIENTED_EDGE ( 'NONE', *, *, #2212, .T. ) ;
#3255 = CARTESIAN_POINT ( 'NONE',  ( -74.00000000204840944, 44.30836144126053000, 25.81189881250000795 ) ) ;
#3256 = CARTESIAN_POINT ( 'NONE',  ( 2.500000000000000000, 0.000000000000000000, -2.968018054819144158 ) ) ;
#3257 = DIRECTION ( 'NONE',  ( -1.000000000000000000, -0.000000000000000000, -0.000000000000000000 ) ) ;
#3258 = CARTESIAN_POINT ( 'NONE',  ( 20.57387831814119750, 55.01735003982987138, 0.01969578267603667651 ) ) ;
#3259 = DIRECTION ( 'NONE',  ( 1.000000000000000000, 0.000000000000000000, 0.000000000000000000 ) ) ;
#3260 = CARTESIAN_POINT ( 'NONE',  ( -75.00000000000001421, 42.56479188213557308, 21.68791366326873060 ) ) ;
#3261 = CIRCLE ( 'NONE', #6367, 1.500000000000001332 ) ;
#3262 = EDGE_LOOP ( 'NONE', ( #1813, #3251, #4411, #11101 ) ) ;
#3263 = CARTESIAN_POINT ( 'NONE',  ( 39.99999999999999289, 55.00000000000000000, -24.99999999999999645 ) ) ;
#3264 = VECTOR ( 'NONE', #3560, 1000.000000000000000 ) ;
#3265 = CARTESIAN_POINT ( 'NONE',  ( -19.59602372284622618, 68.34451306940553650, 16.25656885606184332 ) ) ;
#3266 = VERTEX_POINT ( 'NONE', #9912 ) ;
#3267 = CARTESIAN_POINT ( 'NONE',  ( 3.547974465258201704, 34.60888357062293608, -5.107040723657290116 ) ) ;
#3268 = CARTESIAN_POINT ( 'NONE',  ( -7.668535110823559542, 60.36516981310766283, -12.95174721521620853 ) ) ;
#3269 = CARTESIAN_POINT ( 'NONE',  ( -80.00000000000001421, 71.97056274847716395, 3.371917795327861178E-06 ) ) ;
#3270 = CARTESIAN_POINT ( 'NONE',  ( -25.21223637683726793, 54.34188354068985660, 4.967192001377610744 ) ) ;
#3271 = ORIENTED_EDGE ( 'NONE', *, *, #9932, .T. ) ;
#3272 = CARTESIAN_POINT ( 'NONE',  ( -79.25000000204838102, 80.81189881250001861, -10.69163855873949132 ) ) ;
#3273 = CARTESIAN_POINT ( 'NONE',  ( -80.00000000000002842, 54.99999999999998579, 15.47056612039490986 ) ) ;
#3274 = EDGE_CURVE ( 'NONE', #11230, #1850, #6630, .T. ) ;
#3275 =( NAMED_UNIT ( * ) SI_UNIT ( $, .STERADIAN. ) SOLID_ANGLE_UNIT ( ) );
#3276 = CIRCLE ( 'NONE', #9782, 5.000000000000000888 ) ;
#3277 = LINE ( 'NONE', #5929, #5493 ) ;
#3278 = CIRCLE ( 'NONE', #11311, 4.999999999999997335 ) ;
#3279 = CARTESIAN_POINT ( 'NONE',  ( -54.37536708495734672, 61.59341897336967264, 2.358744290958179057 ) ) ;
#3280 = VERTEX_POINT ( 'NONE', #686 ) ;
#3281 = CARTESIAN_POINT ( 'NONE',  ( -18.73741402030934111, 64.90551912913463184, 18.53518525054827393 ) ) ;
#3282 = AXIS2_PLACEMENT_3D ( 'NONE', #6063, #758, #1725 ) ;
#3283 = CARTESIAN_POINT ( 'NONE',  ( 6.058385820703728442, 34.79737119409461599, 6.139092558150637480 ) ) ;
#3284 = CARTESIAN_POINT ( 'NONE',  ( 1.653121499799245164, -4.819072548984015825, -0.05140428708383163597 ) ) ;
#3285 = EDGE_CURVE ( 'NONE', #11173, #9573, #8534, .T. ) ;
#3286 = CARTESIAN_POINT ( 'NONE',  ( -78.59375000204839523, 55.00000000000000000, 25.81189881249999729 ) ) ;
#3287 = LINE ( 'NONE', #8977, #5352 ) ;
#3288 = CARTESIAN_POINT ( 'NONE',  ( -76.15625000204839523, 73.25176868561975141, -18.25176868561974430 ) ) ;
#3289 = EDGE_LOOP ( 'NONE', ( #1388, #922, #144, #8606 ) ) ;
#3290 = CARTESIAN_POINT ( 'NONE',  ( -72.03125000409679046, 44.64466094067262958, 25.00000000000001066 ) ) ;
#3291 = FACE_BOUND ( 'NONE', #4819, .T. ) ;
#3292 = AXIS2_PLACEMENT_3D ( 'NONE', #8167, #11808, #3434 ) ;
#3293 = VERTEX_POINT ( 'NONE', #8010 ) ;
#3294 = CARTESIAN_POINT ( 'NONE',  ( -17.59602449223222109, 68.34579465778965357, 16.25793134507749826 ) ) ;
#3295 = CARTESIAN_POINT ( 'NONE',  ( -75.21875000204839523, 36.74823131438024859, -18.25176868561973720 ) ) ;
#3296 = CARTESIAN_POINT ( 'NONE',  ( 47.00000000000000000, 51.46446609406726935, -3.535533905932738197 ) ) ;
#3297 = CARTESIAN_POINT ( 'NONE',  ( -73.43750000000008527, 72.67766952966360350, 17.67766952966359284 ) ) ;
#3298 = PRODUCT_DEFINITION ( 'UNKNOWN', '', #3160, #7033 ) ;
#3299 = VERTEX_POINT ( 'NONE', #10572 ) ;
#3300 = DIRECTION ( 'NONE',  ( -1.000000000000000000, -0.000000000000000000, -0.000000000000000000 ) ) ;
#3301 = EDGE_CURVE ( 'NONE', #11519, #1419, #628, .T. ) ;
#3302 = CARTESIAN_POINT ( 'NONE',  ( -75.40625000000000000, 65.35533905932737753, -24.99999999999999645 ) ) ;
#3303 = CARTESIAN_POINT ( 'NONE',  ( 36.99999999999999289, 55.00000000000000000, 22.00000000000000000 ) ) ;
#3304 = ORIENTED_EDGE ( 'NONE', *, *, #9157, .T. ) ;
#3305 = DIRECTION ( 'NONE',  ( -1.000000000000000000, -0.000000000000000000, -0.000000000000000000 ) ) ;
#3306 = PRODUCT_DEFINITION_CONTEXT ( 'detailed design', #10813, 'design' ) ;
#3307 = VERTEX_POINT ( 'NONE', #6046 ) ;
#3308 = CARTESIAN_POINT ( 'NONE',  ( -62.41739093814645400, 50.54543071709656488, 5.426587404619046318 ) ) ;
#3309 = EDGE_CURVE ( 'NONE', #11604, #8631, #9678, .T. ) ;
#3310 = EDGE_CURVE ( 'NONE', #1626, #5647, #1364, .T. ) ;
#3311 = CARTESIAN_POINT ( 'NONE',  ( -78.00000000000002842, 50.75735931288069480, 12.72792543327563131 ) ) ;
#3312 = CARTESIAN_POINT ( 'NONE',  ( -3.000000000000000000, 0.000000000000000000, -0.02539999999999996774 ) ) ;
#3313 = CARTESIAN_POINT ( 'NONE',  ( 52.99999999999999289, 93.00000000000000000, -4.256777005095426300E-16 ) ) ;
#3314 = CARTESIAN_POINT ( 'NONE',  ( -78.12500000204839523, 44.30836144126049447, -25.81189881249999019 ) ) ;
#3315 = ORIENTED_EDGE ( 'NONE', *, *, #5711, .T. ) ;
#3316 = CARTESIAN_POINT ( 'NONE',  ( -78.78125000204839523, 73.25176868561975141, 18.25176868561974075 ) ) ;
#3317 = EDGE_CURVE ( 'NONE', #3221, #5447, #4516, .T. ) ;
#3318 = LINE ( 'NONE', #6985, #11504 ) ;
#3319 = CARTESIAN_POINT ( 'NONE',  ( -75.00000000000000000, 55.00000000000000711, -29.00000000000000355 ) ) ;
#3320 = CARTESIAN_POINT ( 'NONE',  ( -5.204882849839850500, 55.00196753710881836, -0.004080773591198232075 ) ) ;
#3321 = CARTESIAN_POINT ( 'NONE',  ( -78.00000000000001421, 67.72792206135787296, -4.242637315201482906 ) ) ;
#3322 = VERTEX_POINT ( 'NONE', #1346 ) ;
#3323 = DIRECTION ( 'NONE',  ( 0.000000000000000000, 0.000000000000000000, 1.000000000000000000 ) ) ;
#3324 = CARTESIAN_POINT ( 'NONE',  ( -52.82691659388441252, 75.69008924411679118, 4.122156975067814422 ) ) ;
#3325 = ORIENTED_EDGE ( 'NONE', *, *, #4193, .T. ) ;
#3326 = CARTESIAN_POINT ( 'NONE',  ( -18.92935731264207888, 68.34494026553466028, 16.25702301906597569 ) ) ;
#3327 = CARTESIAN_POINT ( 'NONE',  ( -9.410607229192429202, 63.88828574158252138, -10.82921152398832021 ) ) ;
#3328 = LINE ( 'NONE', #6277, #748 ) ;
#3329 = EDGE_LOOP ( 'NONE', ( #10951, #3164, #782, #8582 ) ) ;
#3330 = CARTESIAN_POINT ( 'NONE',  ( -74.28125000000000000, 30.00000000000000355, -10.35533905932738108 ) ) ;
#3331 = CARTESIAN_POINT ( 'NONE',  ( 39.99999999999999289, 39.99999999999999289, -19.99999999999999289 ) ) ;
#3332 = VECTOR ( 'NONE', #5999, 1000.000000000000000 ) ;
#3333 = DIRECTION ( 'NONE',  ( 0.000000000000000000, 0.000000000000000000, 1.000000000000000000 ) ) ;
#3334 = CARTESIAN_POINT ( 'NONE',  ( 53.00000000000000000, 47.00000000000000711, 6.000000000000000000 ) ) ;
#3335 = CARTESIAN_POINT ( 'NONE',  ( -25.89008532269601659, 53.17435935992097029, 6.801947025163535443 ) ) ;
#3336 = ORIENTED_EDGE ( 'NONE', *, *, #10323, .F. ) ;
#3337 = CARTESIAN_POINT ( 'NONE',  ( -46.52239103091250172, 73.32882989972571863, -10.56393531560676102 ) ) ;
#3338 = LINE ( 'NONE', #9690, #5868 ) ;
#3339 = DIRECTION ( 'NONE',  ( 0.000000000000000000, -0.000000000000000000, -1.000000000000000000 ) ) ;
#3340 = LINE ( 'NONE', #1599, #9731 ) ;
#3341 = CARTESIAN_POINT ( 'NONE',  ( -72.03125000204839523, 36.74823131438024859, -18.25176868561973720 ) ) ;
#3342 = ORIENTED_EDGE ( 'NONE', *, *, #589, .F. ) ;
#3343 = CARTESIAN_POINT ( 'NONE',  ( -71.09375000409677625, 80.00000000000001421, -10.35533905932737753 ) ) ;
#3344 = PLANE ( 'NONE',  #3624 ) ;
#3345 = LINE ( 'NONE', #10761, #6555 ) ;
#3346 = CARTESIAN_POINT ( 'NONE',  ( -5.929357825456832209, 64.91315550346766372, -18.55154749960842153 ) ) ;
#3347 = ORIENTED_EDGE ( 'NONE', *, *, #3649, .T. ) ;
#3348 = CARTESIAN_POINT ( 'NONE',  ( -76.90625000204838102, 29.18810118750000271, 4.741568889096522788E-15 ) ) ;
#3349 = CARTESIAN_POINT ( 'NONE',  ( -64.47634457867742697, 52.78883415961983872, 4.496407241981684955 ) ) ;
#3350 = DIRECTION ( 'NONE',  ( 1.000000000000000000, 0.000000000000000000, 0.000000000000000000 ) ) ;
#3351 = VECTOR ( 'NONE', #1109, 1000.000000000000000 ) ;
#3352 = CARTESIAN_POINT ( 'NONE',  ( -34.17314261869798742, 34.29999169977881479, -4.109493429249395646 ) ) ;
#3353 = DIRECTION ( 'NONE',  ( 0.000000000000000000, 0.000000000000000000, 1.000000000000000000 ) ) ;
#3354 = EDGE_CURVE ( 'NONE', #8389, #5247, #11635, .T. ) ;
#3355 = CARTESIAN_POINT ( 'NONE',  ( -75.87500000204839523, 65.69163855873949842, 25.81189881250000440 ) ) ;
#3356 = DIRECTION ( 'NONE',  ( 1.000000000000000000, 6.033820786006286457E-17, -0.000000000000000000 ) ) ;
#3357 = VERTEX_POINT ( 'NONE', #3921 ) ;
#3358 = CARTESIAN_POINT ( 'NONE',  ( 0.000000000000000000, 0.000000000000000000, -2.103846626247716234 ) ) ;
#3359 = VERTEX_POINT ( 'NONE', #5908 ) ;
#3360 = CARTESIAN_POINT ( 'NONE',  ( -27.99986027349028817, 48.52216085064172546, 2.682930977694029551 ) ) ;
#3361 = DIRECTION ( 'NONE',  ( -6.033820786006286457E-17, 1.000000000000000000, 0.000000000000000000 ) ) ;
#3362 = CARTESIAN_POINT ( 'NONE',  ( 39.99999999999999289, 55.00000000000000000, 0.000000000000000000 ) ) ;
#3363 = DIRECTION ( 'NONE',  ( -0.000000000000000000, -0.000000000000000000, -1.000000000000000000 ) ) ;
#3364 = CIRCLE ( 'NONE', #4906, 1.500000000000001332 ) ;
#3365 = CARTESIAN_POINT ( 'NONE',  ( 15.37375454209301395, 71.93308920591223909, -14.05578583284283312 ) ) ;
#3366 = DIRECTION ( 'NONE',  ( 1.000000000000000000, 0.000000000000000000, 0.000000000000000000 ) ) ;
#3367 = EDGE_LOOP ( 'NONE', ( #5483, #7810, #2551, #3347 ) ) ;
#3368 = MECHANICAL_DESIGN_GEOMETRIC_PRESENTATION_REPRESENTATION (  '', ( #8538 ), #11007 ) ;
#3369 = CARTESIAN_POINT ( 'NONE',  ( -77.37500000204838102, 80.81189881250001861, 10.69163855873948599 ) ) ;
#3370 = EDGE_CURVE ( 'NONE', #9755, #5641, #3364, .T. ) ;
#3371 = CARTESIAN_POINT ( 'NONE',  ( -78.00000000000000000, 55.00000000000000000, 21.50000000000000000 ) ) ;
#3372 = CARTESIAN_POINT ( 'NONE',  ( -72.87500000409677625, 55.00000000000000000, -24.99999999999999645 ) ) ;
#3373 = CARTESIAN_POINT ( 'NONE',  ( 17.42607031566902975, 55.00164666455483342, -0.02617539568509523462 ) ) ;
#3374 = DIRECTION ( 'NONE',  ( 0.000000000000000000, 0.000000000000000000, 1.000000000000000000 ) ) ;
#3375 = CIRCLE ( 'NONE', #8550, 1.500000000000001332 ) ;
#3376 = ORIENTED_EDGE ( 'NONE', *, *, #8735, .T. ) ;
#3377 = CARTESIAN_POINT ( 'NONE',  ( -27.71226046275158694, 50.44280945467068022, 2.063697696152629213 ) ) ;
#3378 = EDGE_CURVE ( 'NONE', #2186, #9436, #861, .T. ) ;
#3379 = CARTESIAN_POINT ( 'NONE',  ( -64.51030549024622474, 43.28227691760346119, 17.55408017169854418 ) ) ;
#3380 = EDGE_LOOP ( 'NONE', ( #7030, #10926 ) ) ;
#3381 = CARTESIAN_POINT ( 'NONE',  ( -35.47759590132267249, 36.63029660218667516, -10.58073486798289409 ) ) ;
#3382 = CARTESIAN_POINT ( 'NONE',  ( -32.74394056260254615, 41.05762397541256803, 1.372441782585282155 ) ) ;
#3383 = CARTESIAN_POINT ( 'NONE',  ( -77.28125000204838102, 55.00000000000000000, 25.81189881249999729 ) ) ;
#3384 = CIRCLE ( 'NONE', #8755, 1.500000000000001332 ) ;
#3385 = AXIS2_PLACEMENT_3D ( 'NONE', #9432, #10208, #10143 ) ;
#3386 = ORIENTED_EDGE ( 'NONE', *, *, #8584, .T. ) ;
#3387 = CARTESIAN_POINT ( 'NONE',  ( -79.43750000204838102, 65.69163855873948421, -25.81189881250000440 ) ) ;
#3388 = CARTESIAN_POINT ( 'NONE',  ( 23.47754340821147068, 75.43020022661498558, 5.490793176664390707 ) ) ;
#3389 = FILL_AREA_STYLE ('',( #5882 ) ) ;
#3390 = ORIENTED_EDGE ( 'NONE', *, *, #3458, .T. ) ;
#3391 =( LENGTH_UNIT ( ) NAMED_UNIT ( * ) SI_UNIT ( .MILLI., .METRE. ) );
#3392 = AXIS2_PLACEMENT_3D ( 'NONE', #2232, #6139, #7873 ) ;
#3393 = CARTESIAN_POINT ( 'NONE',  ( 13.70862763294794640, 52.78289059355582680, 4.493706804602685345 ) ) ;
#3394 = CARTESIAN_POINT ( 'NONE',  ( -10.33346892558120800, 59.95411981434817505, -4.954567573143832782 ) ) ;
#3395 =( GEOMETRIC_REPRESENTATION_CONTEXT ( 3 ) GLOBAL_UNCERTAINTY_ASSIGNED_CONTEXT ( ( #5242 ) ) GLOBAL_UNIT_ASSIGNED_CONTEXT ( ( #6220, #5258, #5946 ) ) REPRESENTATION_CONTEXT ( 'NONE', 'WORKASPACE' ) );
#3396 = ORIENTED_EDGE ( 'NONE', *, *, #804, .F. ) ;
#3397 = CARTESIAN_POINT ( 'NONE',  ( -2.855652858599348143, 52.25407377826859801, -20.97791091579992440 ) ) ;
#3398 = FACE_OUTER_BOUND ( 'NONE', #3409, .T. ) ;
#3399 = FACE_OUTER_BOUND ( 'NONE', #836, .T. ) ;
#3400 = EDGE_CURVE ( 'NONE', #567, #7749, #8660, .T. ) ;
#3401 = CARTESIAN_POINT ( 'NONE',  ( -75.00000000000000000, 55.00000000000000000, 0.000000000000000000 ) ) ;
#3402 = CARTESIAN_POINT ( 'NONE',  ( -71.65625000204839523, 73.25176868561975141, -18.25176868561974430 ) ) ;
#3403 = ORIENTED_EDGE ( 'NONE', *, *, #1765, .F. ) ;
#3404 = CARTESIAN_POINT ( 'NONE',  ( -70.87427368927673399, 76.65063840437987608, 12.49999426731031527 ) ) ;
#3405 = FACE_OUTER_BOUND ( 'NONE', #249, .T. ) ;
#3406 = CARTESIAN_POINT ( 'NONE',  ( -66.01541562873828184, 50.16044088320995087, 1.297932126172365752 ) ) ;
#3407 = AXIS2_PLACEMENT_3D ( 'NONE', #7024, #5160, #1320 ) ;
#3408 = CARTESIAN_POINT ( 'NONE',  ( -6.785358873008338954, 67.52118754941005818, -16.88410835930674381 ) ) ;
#3409 = EDGE_LOOP ( 'NONE', ( #10070, #7159, #7399, #383 ) ) ;
#3410 = CARTESIAN_POINT ( 'NONE',  ( -76.43750000204838102, 65.69163855873948421, -25.81189881250000084 ) ) ;
#3411 = CARTESIAN_POINT ( 'NONE',  ( -62.14557957614105277, 54.67521725067852856, 5.000265375653349942 ) ) ;
#3412 = LINE ( 'NONE', #10769, #7255 ) ;
#3413 = CARTESIAN_POINT ( 'NONE',  ( -54.00383531698385298, 74.42670172875287449, 8.047314657126378279 ) ) ;
#3414 = CARTESIAN_POINT ( 'NONE',  ( -78.00000000000001421, 50.75735931288069480, -12.72791868944003824 ) ) ;
#3415 = CARTESIAN_POINT ( 'NONE',  ( -77.37500000204838102, 65.69163855873949842, 25.81189881250000440 ) ) ;
#3416 = CARTESIAN_POINT ( 'NONE',  ( -69.91923606153405046, 50.00000003590698583, -0.0006041109642164819819 ) ) ;
#3417 = EDGE_LOOP ( 'NONE', ( #3620, #10218, #1602, #3403 ) ) ;
#3418 = EDGE_CURVE ( 'NONE', #5411, #6717, #4247, .T. ) ;
#3419 = CARTESIAN_POINT ( 'NONE',  ( -78.00000000000002842, 59.24264068711927678, 14.22792543327563131 ) ) ;
#3420 = ORIENTED_EDGE ( 'NONE', *, *, #10995, .T. ) ;
#3421 = COLOUR_RGB ( '',1.000000000000000000, 0.9490196078431372140, 0.9098039215686274384 ) ;
#3422 = CARTESIAN_POINT ( 'NONE',  ( 23.79370066466821498, 68.61228347134048988, 3.656683429161660115 ) ) ;
#3423 = PLANE ( 'NONE',  #7875 ) ;
#3424 = CARTESIAN_POINT ( 'NONE',  ( 2.287832656137189336, -4.452621892014644978, -6.099999999999998757 ) ) ;
#3425 = CARTESIAN_POINT ( 'NONE',  ( 13.91855488460707058, 70.86244548763734485, -15.28271326984324929 ) ) ;
#3426 = AXIS2_PLACEMENT_3D ( 'NONE', #7010, #6290, #9693 ) ;
#3427 = CARTESIAN_POINT ( 'NONE',  ( 5.000000000000000000, 2.886751345948134428, -5.653418012614792154 ) ) ;
#3428 = AXIS2_PLACEMENT_3D ( 'NONE', #8541, #9314, #324 ) ;
#3429 = ORIENTED_EDGE ( 'NONE', *, *, #1684, .F. ) ;
#3430 = CARTESIAN_POINT ( 'NONE',  ( -74.46875000204839523, 80.81189881250000440, -1.580522963032174394E-15 ) ) ;
#3431 = ADVANCED_FACE ( 'NONE', ( #11571 ), #7966, .T. ) ;
#3432 = CARTESIAN_POINT ( 'NONE',  ( 3.000000000000000000, 3.673940397442059868E-16, -2.617914285714285416 ) ) ;
#3433 = UNCERTAINTY_MEASURE_WITH_UNIT (LENGTH_MEASURE( 1.000000000000000082E-05 ), #11335, 'distance_accuracy_value', 'NONE');
#3434 = DIRECTION ( 'NONE',  ( 0.000000000000000000, 0.000000000000000000, 1.000000000000000000 ) ) ;
#3435 = CARTESIAN_POINT ( 'NONE',  ( 13.57397298349323123, 54.98844360358936001, 0.02356420128931584895 ) ) ;
#3436 = AXIS2_PLACEMENT_3D ( 'NONE', #3879, #8672, #2136 ) ;
#3437 =( NAMED_UNIT ( * ) SI_UNIT ( $, .STERADIAN. ) SOLID_ANGLE_UNIT ( ) );
#3438 = VECTOR ( 'NONE', #539, 1000.000000000000000 ) ;
#3439 = CARTESIAN_POINT ( 'NONE',  ( -75.00000000000001421, 30.35902998560163013, -6.810003371955200890 ) ) ;
#3440 = ORIENTED_EDGE ( 'NONE', *, *, #1274, .T. ) ;
#3441 = CARTESIAN_POINT ( 'NONE',  ( -25.18353888624136516, 51.69772872632766791, 3.768611304527443640 ) ) ;
#3442 = CARTESIAN_POINT ( 'NONE',  ( 19.99999999999996803, -63.00000000000000000, 5.000000000000000000 ) ) ;
#3443 = ORIENTED_EDGE ( 'NONE', *, *, #4044, .T. ) ;
#3444 = CARTESIAN_POINT ( 'NONE',  ( -33.50647601322769731, 34.29967001110087210, -4.109490822278082156 ) ) ;
#3445 = CARTESIAN_POINT ( 'NONE',  ( -51.20617496588531026, 68.98201131862417412, -1.831174229402957820 ) ) ;
#3446 = CARTESIAN_POINT ( 'NONE',  ( -76.43750000204838102, 65.69163855873948421, -25.81189881250000440 ) ) ;
#3447 = ADVANCED_FACE ( 'NONE', ( #6987 ), #11382, .T. ) ;
#3448 = CIRCLE ( 'NONE', #1908, 20.00000000000000355 ) ;
#3449 = EDGE_CURVE ( 'NONE', #3299, #656, #6436, .T. ) ;
#3450 = EDGE_CURVE ( 'NONE', #9962, #7344, #5289, .T. ) ;
#3451 = VERTEX_POINT ( 'NONE', #7408 ) ;
#3452 = CARTESIAN_POINT ( 'NONE',  ( -77.65625000204838102, 80.81189881250000440, -1.580522963032174394E-15 ) ) ;
#3453 = CARTESIAN_POINT ( 'NONE',  ( 24.99999999999999645, 76.00000000000000000, 0.000000000000000000 ) ) ;
#3454 = SURFACE_STYLE_FILL_AREA ( #6282 ) ;
#3455 = ORIENTED_EDGE ( 'NONE', *, *, #8368, .T. ) ;
#3456 = VECTOR ( 'NONE', #11025, 1000.000000000000000 ) ;
#3457 = ADVANCED_FACE ( 'NONE', ( #11096 ), #2845, .T. ) ;
#3458 = EDGE_CURVE ( 'NONE', #6384, #3954, #2966, .T. ) ;
#3459 = FACE_OUTER_BOUND ( 'NONE', #5941, .T. ) ;
#3460 = CARTESIAN_POINT ( 'NONE',  ( 16.03565078256021437, 54.66604247513213011, 4.999734568126702250 ) ) ;
#3461 = CARTESIAN_POINT ( 'NONE',  ( 2.756929297555888780, 54.99406534603833308, -0.0008060267085826582035 ) ) ;
#3462 = EDGE_LOOP ( 'NONE', ( #2129, #11848, #5106, #1990 ) ) ;
#3463 = EDGE_CURVE ( 'NONE', #4456, #11337, #4100, .T. ) ;
#3464 = CARTESIAN_POINT ( 'NONE',  ( -5.697310340841898579, 62.08076523182673867, -19.78924413987668629 ) ) ;
#3465 = CIRCLE ( 'NONE', #7321, 1.500000000000001332 ) ;
#3466 = CARTESIAN_POINT ( 'NONE',  ( -12.81092923270300865, 75.46953867936616689, -5.507006106411301616 ) ) ;
#3467 = CARTESIAN_POINT ( 'NONE',  ( 0.4079457818577022499, -5.537975084925951919, -0.3106000600989376470 ) ) ;
#3468 = CARTESIAN_POINT ( 'NONE',  ( 3.000000000000000000, 0.000000000000000000, 0.000000000000000000 ) ) ;
#3469 = CARTESIAN_POINT ( 'NONE',  ( -72.68750000204839523, 65.69163855873949842, 25.81189881250000440 ) ) ;
#3470 = AXIS2_PLACEMENT_3D ( 'NONE', #162, #1965, #1189 ) ;
#3471 = EDGE_LOOP ( 'NONE', ( #2011, #5130 ) ) ;
#3472 = CARTESIAN_POINT ( 'NONE',  ( -74.56250000409677625, 37.32233047033631124, -17.67766952966368166 ) ) ;
#3473 = CARTESIAN_POINT ( 'NONE',  ( -78.00000000000001421, 67.72792206135787296, 12.72792543327562775 ) ) ;
#3474 = DIRECTION ( 'NONE',  ( -1.000000000000000000, -0.000000000000000000, -0.000000000000000000 ) ) ;
#3475 = CARTESIAN_POINT ( 'NONE',  ( -58.69833756168564065, 56.03204939003842355, 20.99267139547387373 ) ) ;
#3476 = VECTOR ( 'NONE', #9982, 1000.000000000000000 ) ;
#3477 = ORIENTED_EDGE ( 'NONE', *, *, #726, .T. ) ;
#3478 = CIRCLE ( 'NONE', #6160, 2.500000000000000000 ) ;
#3479 = DIRECTION ( 'NONE',  ( 0.000000000000000000, 0.000000000000000000, 1.000000000000000000 ) ) ;
#3480 = ORIENTED_EDGE ( 'NONE', *, *, #4994, .T. ) ;
#3481 = CARTESIAN_POINT ( 'NONE',  ( 53.00000000000000000, 51.46446609406726935, 3.535533905932731091 ) ) ;
#3482 = FACE_OUTER_BOUND ( 'NONE', #11135, .T. ) ;
#3483 = CARTESIAN_POINT ( 'NONE',  ( -78.59375000204839523, 36.74823131438026280, 18.25176868561974786 ) ) ;
#3484 = DIRECTION ( 'NONE',  ( 0.000000000000000000, 0.000000000000000000, -1.000000000000000000 ) ) ;
#3485 = ORIENTED_EDGE ( 'NONE', *, *, #9157, .F. ) ;
#3486 = PLANE ( 'NONE',  #200 ) ;
#3487 = EDGE_LOOP ( 'NONE', ( #2585, #7639, #1360, #3325 ) ) ;
#3488 = CARTESIAN_POINT ( 'NONE',  ( 3.412284745132829311, 65.80390522347528304, 22.54555962154040927 ) ) ;
#3489 = CARTESIAN_POINT ( 'NONE',  ( 5.211360173331719636, 41.40800266049619438, -3.403751673813347089 ) ) ;
#3490 = DIRECTION ( 'NONE',  ( -1.000000000000000000, 0.000000000000000000, 0.000000000000000000 ) ) ;
#3491 = DIRECTION ( 'NONE',  ( -0.000000000000000000, -0.000000000000000000, 1.000000000000000000 ) ) ;
#3492 = CARTESIAN_POINT ( 'NONE',  ( -77.75000000000000000, 55.00000000000000000, 24.99999999999999645 ) ) ;
#3493 = CARTESIAN_POINT ( 'NONE',  ( -71.65625000204838102, 80.81189881250000440, -1.580522963032174394E-15 ) ) ;
#3494 = VERTEX_POINT ( 'NONE', #2240 ) ;
#3495 = CARTESIAN_POINT ( 'NONE',  ( -74.18750000204839523, 65.69163855873949842, 25.81189881250000440 ) ) ;
#3496 = CARTESIAN_POINT ( 'NONE',  ( 0.000000000000000000, 0.000000000000000000, 0.000000000000000000 ) ) ;
#3497 = CARTESIAN_POINT ( 'NONE',  ( -76.71875000409676204, 65.35533905932729226, 25.00000000000008527 ) ) ;
#3498 = CARTESIAN_POINT ( 'NONE',  ( 15.90727646477327717, 54.99834087400687821, 0.02619391509296356210 ) ) ;
#3499 = DIRECTION ( 'NONE',  ( 0.000000000000000000, 0.000000000000000000, 1.000000000000000000 ) ) ;
#3500 = CARTESIAN_POINT ( 'NONE',  ( -75.00000000000000000, 36.04064405738017740, 16.53539858576419519 ) ) ;
#3501 = EDGE_LOOP ( 'NONE', ( #6121, #3561, #7296, #7759 ) ) ;
#3502 = PLANE ( 'NONE',  #8367 ) ;
#3503 = CARTESIAN_POINT ( 'NONE',  ( -2.500000000000000000, 3.061616997868383141E-16, -1.239675197676287643 ) ) ;
#3504 = ORIENTED_EDGE ( 'NONE', *, *, #1032, .T. ) ;
#3505 = CARTESIAN_POINT ( 'NONE',  ( -52.16024998812459756, 75.68979335697233068, 4.122031507855797194 ) ) ;
#3506 = CARTESIAN_POINT ( 'NONE',  ( -75.50000000204840944, 29.18810118750000981, 10.69163855873950020 ) ) ;
#3507 = EDGE_LOOP ( 'NONE', ( #6227, #10207 ) ) ;
#3508 = CARTESIAN_POINT ( 'NONE',  ( -77.00000000000000000, 55.00000000000000000, -24.99999999999999645 ) ) ;
#3509 = LINE ( 'NONE', #3331, #2985 ) ;
#3510 = ORIENTED_EDGE ( 'NONE', *, *, #151, .T. ) ;
#3511 = LINE ( 'NONE', #7126, #2467 ) ;
#3512 = CARTESIAN_POINT ( 'NONE',  ( 24.20135950461900265, 59.84025108871626486, 1.295421926073733410 ) ) ;
#3513 = CARTESIAN_POINT ( 'NONE',  ( -59.91576240004388154, 57.04875898427261660, 6.741986199795334755 ) ) ;
#3514 = VERTEX_POINT ( 'NONE', #5910 ) ;
#3515 = CARTESIAN_POINT ( 'NONE',  ( 16.52229576424834079, 60.50792211291388867, 20.47270680267081389 ) ) ;
#3516 = CARTESIAN_POINT ( 'NONE',  ( -36.14426256656389569, 36.63180902967581432, -10.58010824564746599 ) ) ;
#3517 = DIRECTION ( 'NONE',  ( 0.000000000000000000, 1.000000000000000000, 0.000000000000000000 ) ) ;
#3518 = CARTESIAN_POINT ( 'NONE',  ( -76.62500000409677625, 55.00000000000000000, 24.99999999999999645 ) ) ;
#3519 = DIRECTION ( 'NONE',  ( -0.000000000000000000, -0.000000000000000000, -1.000000000000000000 ) ) ;
#3520 = EDGE_CURVE ( 'NONE', #2575, #9843, #6872, .T. ) ;
#3521 = ORIENTED_EDGE ( 'NONE', *, *, #8531, .T. ) ;
#3522 = DIRECTION ( 'NONE',  ( 0.000000000000000000, 0.000000000000000000, 1.000000000000000000 ) ) ;
#3523 = FACE_OUTER_BOUND ( 'NONE', #334, .T. ) ;
#3524 = LINE ( 'NONE', #5155, #11694 ) ;
#3525 = CARTESIAN_POINT ( 'NONE',  ( -42.96936073659074395, 63.99245613053683712, -19.01383356661934343 ) ) ;
#3526 = EDGE_LOOP ( 'NONE', ( #9424, #10546, #698, #1425, #5062, #11118, #312, #648 ) ) ;
#3527 = DIRECTION ( 'NONE',  ( -0.000000000000000000, -0.000000000000000000, 1.000000000000000000 ) ) ;
#3528 = EDGE_CURVE ( 'NONE', #1709, #4282, #6633, .T. ) ;
#3529 = CARTESIAN_POINT ( 'NONE',  ( -75.00000000000000000, 55.00000000000000000, 25.00000000000000355 ) ) ;
#3530 = ADVANCED_FACE ( 'NONE', ( #2180 ), #9554, .F. ) ;
#3531 = EDGE_LOOP ( 'NONE', ( #106, #7867 ) ) ;
#3532 = DIRECTION ( 'NONE',  ( -0.000000000000000000, -0.000000000000000000, -1.000000000000000000 ) ) ;
#3533 = CARTESIAN_POINT ( 'NONE',  ( 20.29449446700749959, 59.74572742522828861, 1.608070810192847810 ) ) ;
#3534 = CARTESIAN_POINT ( 'NONE',  ( -75.21875000204839523, 36.74823131438024859, -18.25176868561973720 ) ) ;
#3535 = CARTESIAN_POINT ( 'NONE',  ( -77.56250000204838102, 80.81189881250001861, 10.69163855873948599 ) ) ;
#3536 = ORIENTED_EDGE ( 'NONE', *, *, #9673, .F. ) ;
#3537 = FACE_OUTER_BOUND ( 'NONE', #2019, .T. ) ;
#3538 = ORIENTED_EDGE ( 'NONE', *, *, #1824, .T. ) ;
#3539 = CARTESIAN_POINT ( 'NONE',  ( 2.046876773580067255, 51.69375302741990907, -3.765136267534306747 ) ) ;
#3540 = CARTESIAN_POINT ( 'NONE',  ( 6.963661241466286178, 41.00824184081660917, 0.6875629968608463205 ) ) ;
#3541 = CARTESIAN_POINT ( 'NONE',  ( -78.12500000204839523, 29.18810118750000626, -10.69163855873949132 ) ) ;
#3542 =( BOUNDED_CURVE ( )  B_SPLINE_CURVE ( 2, ( #5680, #2071, #9378, #7539, #11288, #2008, #3036, #3154, #4896 ),
 .UNSPECIFIED., .F., .T. ) 
 B_SPLINE_CURVE_WITH_KNOTS ( ( 3, 2, 2, 2, 3 ),
 ( 0.08333333333333339810, 0.1041666666666667546, 0.1250000000000001110, 0.1458333333333334814, 0.1666666666666667962 ),
 .UNSPECIFIED. ) 
 CURVE ( )  GEOMETRIC_REPRESENTATION_ITEM ( )  RATIONAL_B_SPLINE_CURVE ( ( 0.9999999999999997780, 0.9238795325112869605, 1.000000000000000000, 0.9238795325112867385, 1.000000000000000000, 0.9238795325112867385, 1.000000000000000000, 0.9238795325112861834, 1.000000000000000444 ) ) 
 REPRESENTATION_ITEM ( '' )  );
#3543 = LINE ( 'NONE', #1681, #885 ) ;
#3544 =( GEOMETRIC_REPRESENTATION_CONTEXT ( 3 ) GLOBAL_UNCERTAINTY_ASSIGNED_CONTEXT ( ( #394 ) ) GLOBAL_UNIT_ASSIGNED_CONTEXT ( ( #5013, #7644, #3089 ) ) REPRESENTATION_CONTEXT ( 'NONE', 'WORKASPACE' ) );
#3545 = AXIS2_PLACEMENT_3D ( 'NONE', #2311, #9622, #9115 ) ;
#3546 = DIRECTION ( 'NONE',  ( 1.000000000000000000, 0.000000000000000000, 0.000000000000000000 ) ) ;
#3547 = CARTESIAN_POINT ( 'NONE',  ( -73.71875000204839523, 36.74823131438024859, -18.25176868561973720 ) ) ;
#3548 = ORIENTED_EDGE ( 'NONE', *, *, #4766, .F. ) ;
#3549 = FACE_OUTER_BOUND ( 'NONE', #2260, .T. ) ;
#3550 = CARTESIAN_POINT ( 'NONE',  ( -78.68750000409679046, 72.67766952966368876, -17.67766952966368876 ) ) ;
#3551 = EDGE_CURVE ( 'NONE', #849, #1312, #7026, .T. ) ;
#3552 = LINE ( 'NONE', #7223, #3926 ) ;
#3553 = CARTESIAN_POINT ( 'NONE',  ( 53.00000000000000000, 105.0000000000000142, 0.000000000000000000 ) ) ;
#3554 = DIRECTION ( 'NONE',  ( 1.000000000000000000, 0.000000000000000000, 0.000000000000000000 ) ) ;
#3555 = CARTESIAN_POINT ( 'NONE',  ( -27.66451880046085776, 54.99704050659160259, 0.001041102682434957849 ) ) ;
#3556 = CARTESIAN_POINT ( 'NONE',  ( -11.21107213742082109, 69.03605984126116368, -16.94742667234782374 ) ) ;
#3557 = CONICAL_SURFACE ( 'NONE', #10242, 4.999999999999995559, 0.7853981633974530530 ) ;
#3558 = ORIENTED_EDGE ( 'NONE', *, *, #1152, .F. ) ;
#3559 = CARTESIAN_POINT ( 'NONE',  ( -13.51214745100933357, 59.74687554544813395, 1.604952281176790230 ) ) ;
#3560 = DIRECTION ( 'NONE',  ( 0.000000000000000000, 1.000000000000000000, 0.000000000000000000 ) ) ;
#3561 = ORIENTED_EDGE ( 'NONE', *, *, #6847, .T. ) ;
#3562 = CARTESIAN_POINT ( 'NONE',  ( -30.00387656835589212, 35.57275282082603240, 8.046560464864068507 ) ) ;
#3563 = CARTESIAN_POINT ( 'NONE',  ( -74.65625000204838102, 80.81189881250000440, -1.580522963032174394E-15 ) ) ;
#3564 = AXIS2_PLACEMENT_3D ( 'NONE', #11336, #3144, #11573 ) ;
#3565 = ORIENTED_EDGE ( 'NONE', *, *, #10114, .F. ) ;
#3566 = PRODUCT_DEFINITION_SHAPE ( 'NONE', 'NONE',  #4545 ) ;
#3567 = EDGE_CURVE ( 'NONE', #7792, #2110, #8715, .T. ) ;
#3568 = CARTESIAN_POINT ( 'NONE',  ( -76.81250000000007105, 72.67766952966361771, -17.67766952966362126 ) ) ;
#3569 = CARTESIAN_POINT ( 'NONE',  ( -20.50647613538409075, 59.12524989819403487, 20.69783765389080799 ) ) ;
#3570 = CIRCLE ( 'NONE', #9491, 1.500000000000001332 ) ;
#3571 = DIRECTION ( 'NONE',  ( 0.000000000000000000, 0.000000000000000000, 1.000000000000000000 ) ) ;
#3572 = EDGE_CURVE ( 'NONE', #6455, #7832, #9293, .T. ) ;
#3573 = CARTESIAN_POINT ( 'NONE',  ( 21.24062560320400550, 55.01638079892301647, 0.001655951099807092403 ) ) ;
#3574 = ORIENTED_EDGE ( 'NONE', *, *, #2980, .F. ) ;
#3575 = CARTESIAN_POINT ( 'NONE',  ( -59.59556320886013481, 52.94111634316250559, 20.93276532467568174 ) ) ;
#3576 = VECTOR ( 'NONE', #10475, 1000.000000000000000 ) ;
#3577 = CARTESIAN_POINT ( 'NONE',  ( -21.63602683877659771, 62.08561388645346568, 19.80191166437241179 ) ) ;
#3578 = AXIS2_PLACEMENT_3D ( 'NONE', #6476, #11060, #2989 ) ;
#3579 = FACE_OUTER_BOUND ( 'NONE', #3462, .T. ) ;
#3580 = FACE_OUTER_BOUND ( 'NONE', #326, .T. ) ;
#3581 = ADVANCED_FACE ( 'NONE', ( #4830 ), #1835, .T. ) ;
#3582 = ORIENTED_EDGE ( 'NONE', *, *, #10114, .T. ) ;
#3583 = CARTESIAN_POINT ( 'NONE',  ( 0.000000000000000000, 0.000000000000000000, -4.860324802323723326 ) ) ;
#3584 = DIRECTION ( 'NONE',  ( -0.000000000000000000, -0.000000000000000000, -1.000000000000000000 ) ) ;
#3585 = CARTESIAN_POINT ( 'NONE',  ( -43.85119715763887882, 58.30290808985935769, -3.768050382088650618 ) ) ;
#3586 = CIRCLE ( 'NONE', #6459, 1.500000000000001332 ) ;
#3587 = VERTEX_POINT ( 'NONE', #442 ) ;
#3588 = CARTESIAN_POINT ( 'NONE',  ( 7.095683716263478047, 50.00000000000005684, 2.757939276259992832E-15 ) ) ;
#3589 = STYLED_ITEM ( 'NONE', ( #202 ), #1113 ) ;
#3590 = CARTESIAN_POINT ( 'NONE',  ( -65.64956124500029944, 51.95148351646824381, 3.976808671807906315 ) ) ;
#3591 = EDGE_CURVE ( 'NONE', #9484, #9538, #1282, .T. ) ;
#3592 = VERTEX_POINT ( 'NONE', #5797 ) ;
#3593 = CARTESIAN_POINT ( 'NONE',  ( 39.99999999999999289, 55.00000000000000000, 5.249999999999998224 ) ) ;
#3594 = DIRECTION ( 'NONE',  ( -0.000000000000000000, -0.000000000000000000, -1.000000000000000000 ) ) ;
#3595 = CARTESIAN_POINT ( 'NONE',  ( 15.62209821594298198, 57.21425893602940249, 4.494981641845320119 ) ) ;
#3596 = CARTESIAN_POINT ( 'NONE',  ( -75.31250000204839523, 29.18810118750000626, -10.69163855873949309 ) ) ;
#3597 = DIRECTION ( 'NONE',  ( 0.000000000000000000, 1.000000000000000000, 0.000000000000000000 ) ) ;
#3598 = AXIS2_PLACEMENT_3D ( 'NONE', #7146, #11670, #2636 ) ;
#3599 = ORIENTED_EDGE ( 'NONE', *, *, #8805, .T. ) ;
#3600 = CARTESIAN_POINT ( 'NONE',  ( -77.37500000204838102, 80.81189881250001861, 10.69163855873948599 ) ) ;
#3601 = ORIENTED_EDGE ( 'NONE', *, *, #8627, .T. ) ;
#3602 = CARTESIAN_POINT ( 'NONE',  ( 20.93592707265620945, 76.34962308819727639, 13.02666796807690552 ) ) ;
#3603 = CARTESIAN_POINT ( 'NONE',  ( -6.743941583970623377, 63.88657993984631389, -10.82739850970073014 ) ) ;
#3604 = CARTESIAN_POINT ( 'NONE',  ( -75.12500000204838102, 29.18810118750000626, -10.69163855873949132 ) ) ;
#3605 = CARTESIAN_POINT ( 'NONE',  ( -76.81250000409679046, 72.67766952966368876, 17.67766952966368521 ) ) ;
#3606 = CYLINDRICAL_SURFACE ( 'NONE', #7050, 21.50000000000000000 ) ;
#3607 = ORIENTED_EDGE ( 'NONE', *, *, #6827, .T. ) ;
#3608 = EDGE_CURVE ( 'NONE', #5647, #567, #7819, .T. ) ;
#3609 = CARTESIAN_POINT ( 'NONE',  ( -76.53125000409679046, 44.64466094067255142, 24.99999999999992184 ) ) ;
#3610 = CARTESIAN_POINT ( 'NONE',  ( -78.59375000409679046, 80.00000000000001421, -10.35533905932737753 ) ) ;
#3611 = CARTESIAN_POINT ( 'NONE',  ( 53.00000000000000000, 51.46446609406726935, -3.535533905932738197 ) ) ;
#3612 = CARTESIAN_POINT ( 'NONE',  ( 52.99999999999999289, 58.53553390593273065, -3.535533905932738197 ) ) ;
#3613 = CARTESIAN_POINT ( 'NONE',  ( -61.49460156519547382, 54.99554728952567473, 0.005807220347030686396 ) ) ;
#3614 = APPLICATION_PROTOCOL_DEFINITION ( 'draft international standard', 'automotive_design', 1998, #5325 ) ;
#3615 = CARTESIAN_POINT ( 'NONE',  ( -21.37442402976132882, 76.71451586203353656, 3.603759168105849398 ) ) ;
#3616 = CARTESIAN_POINT ( 'NONE',  ( -26.93186442276182291, 50.75324309684062030, 2.644246209326107877 ) ) ;
#3617 = PRESENTATION_LAYER_ASSIGNMENT (  '', '', ( #3801 ) ) ;
#3618 = ORIENTED_EDGE ( 'NONE', *, *, #9071, .T. ) ;
#3619 = CARTESIAN_POINT ( 'NONE',  ( 4.592054218142289201, 3.122278952918447370, -0.3106000600989279326 ) ) ;
#3620 = ORIENTED_EDGE ( 'NONE', *, *, #3551, .F. ) ;
#3621 = CARTESIAN_POINT ( 'NONE',  ( -64.40004821475288566, 41.61990247229329043, 16.30275451258844654 ) ) ;
#3622 = CARTESIAN_POINT ( 'NONE',  ( -77.18750000204839523, 65.69163855873949842, 25.81189881250000440 ) ) ;
#3623 = AXIS2_PLACEMENT_3D ( 'NONE', #4775, #4595, #2745 ) ;
#3624 = AXIS2_PLACEMENT_3D ( 'NONE', #6236, #757, #816 ) ;
#3625 = ORIENTED_EDGE ( 'NONE', *, *, #6915, .F. ) ;
#3626 = CARTESIAN_POINT ( 'NONE',  ( -72.87500000204839523, 65.69163855873949842, 25.81189881250000440 ) ) ;
#3627 = CARTESIAN_POINT ( 'NONE',  ( -6.785358873008338954, 67.52118754941005818, -16.88410835930674381 ) ) ;
#3628 = ORIENTED_EDGE ( 'NONE', *, *, #2500, .F. ) ;
#3629 = DIRECTION ( 'NONE',  ( 0.000000000000000000, 0.000000000000000000, 1.000000000000000000 ) ) ;
#3630 = CARTESIAN_POINT ( 'NONE',  ( 3.335481153117199060, 54.99801350816134260, -0.0001838804729987853024 ) ) ;
#3631 = VECTOR ( 'NONE', #1445, 1000.000000000000000 ) ;
#3632 = ORIENTED_EDGE ( 'NONE', *, *, #5230, .F. ) ;
#3633 = CARTESIAN_POINT ( 'NONE',  ( 15.81093802506984858, 57.74566954809575492, 20.97791266904829044 ) ) ;
#3634 = CARTESIAN_POINT ( 'NONE',  ( -8.214759031591983174, 65.81066618478850216, -18.03675305545087681 ) ) ;
#3635 = CARTESIAN_POINT ( 'NONE',  ( -78.00000000000001421, 67.72792206135787296, -4.242637315201482906 ) ) ;
#3636 = CARTESIAN_POINT ( 'NONE',  ( -48.90475262238859244, 59.99999999999997158, -9.564595459368971197E-12 ) ) ;
#3637 = DIRECTION ( 'NONE',  ( -1.000000000000000000, -0.000000000000000000, -0.000000000000000000 ) ) ;
#3638 = DIRECTION ( 'NONE',  ( 0.000000000000000000, 0.000000000000000000, 1.000000000000000000 ) ) ;
#3639 = ORIENTED_EDGE ( 'NONE', *, *, #1838, .T. ) ;
#3640 = ADVANCED_FACE ( 'NONE', ( #11277 ), #4917, .T. ) ;
#3641 = DIRECTION ( 'NONE',  ( -1.000000000000000000, -0.000000000000000000, -0.000000000000000000 ) ) ;
#3642 = CARTESIAN_POINT ( 'NONE',  ( -19.99785218025166600, 55.00127463874410694, 0.001534684918545882936 ) ) ;
#3643 = CARTESIAN_POINT ( 'NONE',  ( -46.95981180409334854, 59.74564377627622491, -1.608358621211970263 ) ) ;
#3644 = AXIS2_PLACEMENT_3D ( 'NONE', #6082, #548, #4039 ) ;
#3645 = EDGE_CURVE ( 'NONE', #430, #723, #11217, .T. ) ;
#3646 = CARTESIAN_POINT ( 'NONE',  ( -80.00000000000002842, 50.75735931288069480, 11.22792543327563131 ) ) ;
#3647 = VECTOR ( 'NONE', #10191, 1000.000000000000000 ) ;
#3648 = CARTESIAN_POINT ( 'NONE',  ( -74.56250000409677625, 37.32233047033631124, -17.67766952966368166 ) ) ;
#3649 = EDGE_CURVE ( 'NONE', #30, #9521, #11261, .T. ) ;
#3650 = EDGE_LOOP ( 'NONE', ( #10736, #9393 ) ) ;
#3651 = CARTESIAN_POINT ( 'NONE',  ( 2.449293598294706513E-15, 50.00000000000000000, -20.00000000000000000 ) ) ;
#3652 = AXIS2_PLACEMENT_3D ( 'NONE', #781, #5353, #10726 ) ;
#3653 = CARTESIAN_POINT ( 'NONE',  ( -78.00000000000002842, 54.99999999999998579, 18.47056612039490986 ) ) ;
#3654 = DIRECTION ( 'NONE',  ( 0.000000000000000000, 0.000000000000000000, -1.000000000000000000 ) ) ;
#3655 = CARTESIAN_POINT ( 'NONE',  ( -73.71875000204839523, 36.74823131438024859, -18.25176868561973720 ) ) ;
#3656 = CARTESIAN_POINT ( 'NONE',  ( -80.00000000000001421, 54.99999999999998579, -8.485278002320759683 ) ) ;
#3657 = ORIENTED_EDGE ( 'NONE', *, *, #8008, .T. ) ;
#3658 = CARTESIAN_POINT ( 'NONE',  ( -74.46875000204839523, 80.81189881250000440, -1.580522963032174394E-15 ) ) ;
#3659 = CIRCLE ( 'NONE', #3847, 3.000000000000000000 ) ;
#3660 = AXIS2_PLACEMENT_3D ( 'NONE', #296, #6611, #1317 ) ;
#3661 = ORIENTED_EDGE ( 'NONE', *, *, #10581, .F. ) ;
#3662 = CARTESIAN_POINT ( 'NONE',  ( 2.148233841220928753, 65.58248926441827109, 22.64989133859231885 ) ) ;
#3663 = CARTESIAN_POINT ( 'NONE',  ( -20.16981924998567877, 57.75067501206415699, 13.79995037456313334 ) ) ;
#3664 = CARTESIAN_POINT ( 'NONE',  ( -77.56250000204839523, 80.81189881250000440, -10.69163855873948954 ) ) ;
#3665 = CARTESIAN_POINT ( 'NONE',  ( -79.06250000000002842, 37.32233047033633966, 17.67766952966367100 ) ) ;
#3666 = DIRECTION ( 'NONE',  ( -0.8191520442889885789, 1.003171929053520802E-16, 0.5735764363510507113 ) ) ;
#3667 = AXIS2_PLACEMENT_3D ( 'NONE', #5628, #156, #9508 ) ;
#3668 = ORIENTED_EDGE ( 'NONE', *, *, #9507, .T. ) ;
#3669 = DIRECTION ( 'NONE',  ( 2.126576849575776229E-17, 0.9848077530122080203, -0.1736481776669307198 ) ) ;
#3670 = CARTESIAN_POINT ( 'NONE',  ( -75.12500000409677625, 55.00000000000000000, 24.99999999999999645 ) ) ;
#3671 = DIRECTION ( 'NONE',  ( 0.000000000000000000, 0.000000000000000000, 1.000000000000000000 ) ) ;
#3672 = ADVANCED_FACE ( 'NONE', ( #10385 ), #8731, .T. ) ;
#3673 = CARTESIAN_POINT ( 'NONE',  ( -39.90973890762001020, 55.00092042771588297, -0.009673943807180659937 ) ) ;
#3674 = APPLICATION_PROTOCOL_DEFINITION ( 'draft international standard', 'automotive_design', 1998, #4944 ) ;
#3675 = CIRCLE ( 'NONE', #7294, 1.500000000000001332 ) ;
#3676 = CARTESIAN_POINT ( 'NONE',  ( -20.71225445595675296, 76.16273347894681933, 6.021655603152394676 ) ) ;
#3677 = CARTESIAN_POINT ( 'NONE',  ( 47.00000000000000000, 55.00000000000000000, 0.000000000000000000 ) ) ;
#3678 = EDGE_LOOP ( 'NONE', ( #9903, #2707, #1224, #1595, #9444, #8777 ) ) ;
#3679 = DIRECTION ( 'NONE',  ( 0.000000000000000000, 1.000000000000000000, 0.000000000000000000 ) ) ;
#3680 = EDGE_CURVE ( 'NONE', #10987, #5713, #1268, .T. ) ;
#3681 = VERTEX_POINT ( 'NONE', #4463 ) ;
#3682 = CARTESIAN_POINT ( 'NONE',  ( -19.00387657603030078, 69.86840152515847535, 14.86901714484747750 ) ) ;
#3683 = CARTESIAN_POINT ( 'NONE',  ( -72.59375000204838102, 36.74823131438026280, 18.25176868561974786 ) ) ;
#3684 = ORIENTED_EDGE ( 'NONE', *, *, #1024, .F. ) ;
#3685 = CARTESIAN_POINT ( 'NONE',  ( -74.84375000204839523, 73.25176868561975141, -18.25176868561974430 ) ) ;
#3686 = CARTESIAN_POINT ( 'NONE',  ( -37.18898618307433424, 44.43582214169357769, -18.32873044267784479 ) ) ;
#3687 = SHAPE_REPRESENTATION_RELATIONSHIP ( 'NONE' , 'NONE' ,  #11597, #2413 ) ;
#3688 = ORIENTED_EDGE ( 'NONE', *, *, #4934, .F. ) ;
#3689 = DIRECTION ( 'NONE',  ( 0.000000000000000000, 1.000000000000000000, 0.000000000000000000 ) ) ;
#3690 = CARTESIAN_POINT ( 'NONE',  ( 18.09282150389694976, 54.98959524075147698, -0.01273383307231591190 ) ) ;
#3691 = ORIENTED_EDGE ( 'NONE', *, *, #11404, .F. ) ;
#3692 = CARTESIAN_POINT ( 'NONE',  ( -29.92935756904273603, 34.87299855483264110, 6.108044681958789468 ) ) ;
#3693 = CARTESIAN_POINT ( 'NONE',  ( -20.73741325422386339, 64.90628579765783002, 18.53688757488948369 ) ) ;
#3694 = CARTESIAN_POINT ( 'NONE',  ( 5.000000000000000888, 0.000000000000000000, 0.000000000000000000 ) ) ;
#3695 = DIRECTION ( 'NONE',  ( 0.000000000000000000, 0.000000000000000000, -1.000000000000000000 ) ) ;
#3696 = CARTESIAN_POINT ( 'NONE',  ( 3.000000000000000000, 3.673940397442059868E-16, -0.8895714285714284575 ) ) ;
#3697 = CARTESIAN_POINT ( 'NONE',  ( 2.500000000000000000, 0.000000000000000000, -2.968018054819144158 ) ) ;
#3698 = ORIENTED_EDGE ( 'NONE', *, *, #4340, .F. ) ;
#3699 = CARTESIAN_POINT ( 'NONE',  ( 39.99999999999999289, 55.00000000000000000, -24.99999999999999645 ) ) ;
#3700 = CARTESIAN_POINT ( 'NONE',  ( -28.57385868769931747, 55.01273333077524086, -0.01040445938396371457 ) ) ;
#3701 = CARTESIAN_POINT ( 'NONE',  ( -62.13034108455730120, 51.94914922404619517, 3.974862913485895266 ) ) ;
#3702 = DIRECTION ( 'NONE',  ( 0.000000000000000000, 0.000000000000000000, 1.000000000000000000 ) ) ;
#3703 = LINE ( 'NONE', #7430, #10067 ) ;
#3704 = EDGE_LOOP ( 'NONE', ( #4229, #10467 ) ) ;
#3705 = FACE_OUTER_BOUND ( 'NONE', #2536, .T. ) ;
#3706 = CIRCLE ( 'NONE', #4482, 2.500000000000000000 ) ;
#3707 = DIRECTION ( 'NONE',  ( 1.000000000000000000, 0.000000000000000000, 0.000000000000000000 ) ) ;
#3708 = DIRECTION ( 'NONE',  ( 0.000000000000000000, -1.000000000000000000, 0.000000000000000000 ) ) ;
#3709 = CARTESIAN_POINT ( 'NONE',  ( -71.93750000204838102, 65.69163855873948421, -25.81189881250000440 ) ) ;
#3710 = CARTESIAN_POINT ( 'NONE',  ( -75.59375000204839523, 36.74823131438026280, 18.25176868561974786 ) ) ;
#3711 = ORIENTED_EDGE ( 'NONE', *, *, #6362, .F. ) ;
#3712 = CARTESIAN_POINT ( 'NONE',  ( -75.68750000204839523, 65.69163855873949842, 25.81189881250000440 ) ) ;
#3713 = ORIENTED_EDGE ( 'NONE', *, *, #8804, .F. ) ;
#3714 = CARTESIAN_POINT ( 'NONE',  ( 6.317087443011592640, 50.00000000000001421, -0.6593808601074064857 ) ) ;
#3715 = SHAPE_REPRESENTATION ( 'perforated grinding plate', ( #4738 ), #2442 ) ;
#3716 = CARTESIAN_POINT ( 'NONE',  ( 19.87282930741283948, 63.62205004655174889, 11.21167653978275958 ) ) ;
#3717 = CARTESIAN_POINT ( 'NONE',  ( -78.03125000204839523, 36.74823131438024859, -18.25176868561973720 ) ) ;
#3718 = CARTESIAN_POINT ( 'NONE',  ( -75.00000000000000000, 66.33456766258404969, -23.06271704340218065 ) ) ;
#3719 = ADVANCED_FACE ( 'NONE', ( #5184 ), #6932, .F. ) ;
#3720 = CARTESIAN_POINT ( 'NONE',  ( 14.99999999999999645, 5.000000000000000000, 20.00000000000000000 ) ) ;
#3721 = ORIENTED_EDGE ( 'NONE', *, *, #798, .T. ) ;
#3722 = CARTESIAN_POINT ( 'NONE',  ( -79.06250000000001421, 37.32233047033631124, 17.67766952966369232 ) ) ;
#3723 = CARTESIAN_POINT ( 'NONE',  ( -73.06250000204840944, 80.81189881250001861, -10.69163855873949132 ) ) ;
#3724 = DIRECTION ( 'NONE',  ( 0.000000000000000000, 0.000000000000000000, 1.000000000000000000 ) ) ;
#3725 = CARTESIAN_POINT ( 'NONE',  ( -50.71441498082971577, 54.99195842427500480, -0.003607703250841377916 ) ) ;
#3726 = APPLICATION_PROTOCOL_DEFINITION ( 'draft international standard', 'automotive_design', 1998, #10282 ) ;
#3727 = CARTESIAN_POINT ( 'NONE',  ( -18.57601780462385577, 74.41890655751923589, 10.34450647405109081 ) ) ;
#3728 = CARTESIAN_POINT ( 'NONE',  ( -2.500000000000000000, 3.061616997868383141E-16, -6.099999999999999645 ) ) ;
#3729 = ORIENTED_EDGE ( 'NONE', *, *, #6830, .F. ) ;
#3730 = DIRECTION ( 'NONE',  ( -1.000000000000000000, 0.000000000000000000, 0.000000000000000000 ) ) ;
#3731 = EDGE_CURVE ( 'NONE', #2912, #2858, #11488, .T. ) ;
#3732 = CARTESIAN_POINT ( 'NONE',  ( -78.00000000000001421, 42.27207793864211283, -12.72791868944003824 ) ) ;
#3733 = VERTEX_POINT ( 'NONE', #2601 ) ;
#3734 = CARTESIAN_POINT ( 'NONE',  ( -65.80895658223876410, 38.19798843649414977, 12.92520887581758693 ) ) ;
#3735 = CARTESIAN_POINT ( 'NONE',  ( -73.81250000204839523, 29.18810118750000626, -10.69163855873949309 ) ) ;
#3736 = ORIENTED_EDGE ( 'NONE', *, *, #4826, .T. ) ;
#3737 = CARTESIAN_POINT ( 'NONE',  ( -75.78125000204838102, 55.00000000000000000, 25.81189881249999729 ) ) ;
#3738 = CARTESIAN_POINT ( 'NONE',  ( -31.30269415623623885, 33.99224428815358579, -1.031667027462585207 ) ) ;
#3739 = SURFACE_SIDE_STYLE ('',( #7407 ) ) ;
#3740 = EDGE_CURVE ( 'NONE', #10654, #9231, #6637, .T. ) ;
#3741 = CARTESIAN_POINT ( 'NONE',  ( -60.73530621856283318, 48.89645762657089278, 20.10868697360108115 ) ) ;
#3742 = ORIENTED_EDGE ( 'NONE', *, *, #11689, .F. ) ;
#3743 = CARTESIAN_POINT ( 'NONE',  ( -13.15402772192483383, 59.74639309637463924, -1.606196551478056955 ) ) ;
#3744 = CARTESIAN_POINT ( 'NONE',  ( -4.188986194789085182, 52.25407379690145859, -20.98118322582191908 ) ) ;
#3745 = AXIS2_PLACEMENT_3D ( 'NONE', #2552, #9853, #5139 ) ;
#3746 = ORIENTED_EDGE ( 'NONE', *, *, #6842, .T. ) ;
#3747 = CARTESIAN_POINT ( 'NONE',  ( -30.78535887075297595, 34.20700043619147124, 3.085051459701278365 ) ) ;
#3748 = CARTESIAN_POINT ( 'NONE',  ( -43.78535878948660098, 60.10716095388539060, -20.39140800440753054 ) ) ;
#3749 = DIRECTION ( 'NONE',  ( -1.000000000000000000, -0.000000000000000000, -0.000000000000000000 ) ) ;
#3750 = CARTESIAN_POINT ( 'NONE',  ( 5.000000000000000000, -2.417244626924489381, -5.788952927922133895 ) ) ;
#3751 = EDGE_CURVE ( 'NONE', #2443, #241, #5302, .T. ) ;
#3752 = AXIS2_PLACEMENT_3D ( 'NONE', #10313, #4817, #5785 ) ;
#3753 = CYLINDRICAL_SURFACE ( 'NONE', #9172, 24.99999999999999645 ) ;
#3754 = CARTESIAN_POINT ( 'NONE',  ( -72.50000000000000000, 55.00000000000000000, -24.99999999999999645 ) ) ;
#3755 = EDGE_LOOP ( 'NONE', ( #7658, #7752, #4094, #4499, #2958, #6333, #5816, #5791, #8161, #11760, #11701, #8806, #3684, #11318 ) ) ;
#3756 = DIRECTION ( 'NONE',  ( 0.000000000000000000, 0.000000000000000000, 1.000000000000000000 ) ) ;
#3757 = CARTESIAN_POINT ( 'NONE',  ( -54.71441367628058572, 54.99501360422757301, -0.002467102893749668121 ) ) ;
#3758 = CARTESIAN_POINT ( 'NONE',  ( -45.59944951615121056, 59.24594800971062369, -2.645521645423703383 ) ) ;
#3759 = CARTESIAN_POINT ( 'NONE',  ( 53.00000000000000000, 47.00000000000000711, 0.000000000000000000 ) ) ;
#3760 = PRODUCT ( 'Cast Iron Barrel & Hopper Casing', 'Cast Iron Barrel & Hopper Casing', '', ( #9119 ) ) ;
#3761 = CONICAL_SURFACE ( 'NONE', #5303, 4.999999999999995559, 0.7853981633974530530 ) ;
#3762 = FACE_OUTER_BOUND ( 'NONE', #7978, .T. ) ;
#3763 = CARTESIAN_POINT ( 'NONE',  ( -8.874841564931038818, 58.60437997257135834, -6.013803112307263277 ) ) ;
#3764 = ORIENTED_EDGE ( 'NONE', *, *, #9433, .F. ) ;
#3765 = DIRECTION ( 'NONE',  ( 1.000000000000000000, 0.000000000000000000, 0.000000000000000000 ) ) ;
#3766 = DIRECTION ( 'NONE',  ( 0.000000000000000000, 0.000000000000000000, 1.000000000000000000 ) ) ;
#3767 = DIRECTION ( 'NONE',  ( -0.8191520442889885789, 1.003171929053520802E-16, 0.5735764363510507113 ) ) ;
#3768 = DIRECTION ( 'NONE',  ( -1.000000000000000000, 0.000000000000000000, 0.000000000000000000 ) ) ;
#3769 = CARTESIAN_POINT ( 'NONE',  ( 2.782474192756827142E-15, 65.42943686846950868, -22.72062601704910634 ) ) ;
#3770 = CARTESIAN_POINT ( 'NONE',  ( -75.40625000204838102, 29.18810118750000271, 4.741568889096522788E-15 ) ) ;
#3771 = ORIENTED_EDGE ( 'NONE', *, *, #6458, .T. ) ;
#3772 = VECTOR ( 'NONE', #6533, 1000.000000000000000 ) ;
#3773 = CARTESIAN_POINT ( 'NONE',  ( -77.00000000204838102, 44.30836144126053000, 25.81189881250000795 ) ) ;
#3774 = ORIENTED_EDGE ( 'NONE', *, *, #6456, .T. ) ;
#3775 = CARTESIAN_POINT ( 'NONE',  ( 25.22669093968800880, 79.94582849343181863, -1.700159177187467563 ) ) ;
#3776 = CIRCLE ( 'NONE', #9123, 1.500000000000001332 ) ;
#3777 = CARTESIAN_POINT ( 'NONE',  ( -30.66480670352544635, 40.98593724095160695, 0.0004245934155297764051 ) ) ;
#3778 = CARTESIAN_POINT ( 'NONE',  ( -79.25000000204839523, 65.69163855873948421, -25.81189881250000084 ) ) ;
#3779 = CARTESIAN_POINT ( 'NONE',  ( -75.00000000000000000, 73.68484416130073100, -17.40076935087584076 ) ) ;
#3780 = DIRECTION ( 'NONE',  ( 0.000000000000000000, 0.000000000000000000, 1.000000000000000000 ) ) ;
#3781 = CIRCLE ( 'NONE', #895, 1.500000000000001332 ) ;
#3782 = VERTEX_POINT ( 'NONE', #7109 ) ;
#3783 = CARTESIAN_POINT ( 'NONE',  ( -78.21875000000001421, 80.00000000000001421, -10.35533905932737753 ) ) ;
#3784 = CARTESIAN_POINT ( 'NONE',  ( -78.31250000409679046, 72.67766952966368876, 17.67766952966368521 ) ) ;
#3785 = CARTESIAN_POINT ( 'NONE',  ( -78.00000000000002842, 46.51471862576140381, 8.485284746156354529 ) ) ;
#3786 = FACE_BOUND ( 'NONE', #11441, .T. ) ;
#3787 = CARTESIAN_POINT ( 'NONE',  ( -52.75694149779237563, 54.99300116554260853, -0.007378550177579538093 ) ) ;
#3788 = DIRECTION ( 'NONE',  ( 1.000000000000000000, 0.000000000000000000, 0.000000000000000000 ) ) ;
#3789 = CIRCLE ( 'NONE', #3407, 1.500000000000001332 ) ;
#3790 = CARTESIAN_POINT ( 'NONE',  ( -19.43088458554904108, 75.10954819156191320, -8.928210389664046787 ) ) ;
#3791 = CARTESIAN_POINT ( 'NONE',  ( -4.999999999999999112, 0.4881033300985035961, -6.099999999999999645 ) ) ;
#3792 = EDGE_LOOP ( 'NONE', ( #10616, #3016, #10718 ) ) ;
#3793 = CARTESIAN_POINT ( 'NONE',  ( -79.25000000000000000, 55.00000000000000000, 24.99999999999999645 ) ) ;
#3794 = FACE_OUTER_BOUND ( 'NONE', #10488, .T. ) ;
#3795 = ADVANCED_FACE ( 'NONE', ( #6208 ), #2420, .F. ) ;
#3796 = ORIENTED_EDGE ( 'NONE', *, *, #2416, .F. ) ;
#3797 = CARTESIAN_POINT ( 'NONE',  ( -19.59602372284622618, 68.34451306940553650, 16.25656885606184332 ) ) ;
#3798 = CARTESIAN_POINT ( 'NONE',  ( -73.90625000204838102, 29.18810118750000271, 4.741568889096522788E-15 ) ) ;
#3799 = CARTESIAN_POINT ( 'NONE',  ( -76.53125000000004263, 79.99999999999990052, 10.35533905932733312 ) ) ;
#3800 = CARTESIAN_POINT ( 'NONE',  ( -7.969360823174009845, 70.58422527244209732, -14.12522777056770629 ) ) ;
#3801=STYLED_ITEM('',(#11895),#4897);
#3802 = CARTESIAN_POINT ( 'NONE',  ( 0.000000000000000000, 0.000000000000000000, -0.3755037691048591086 ) ) ;
#3803 = ORIENTED_EDGE ( 'NONE', *, *, #3019, .F. ) ;
#3804 = CARTESIAN_POINT ( 'NONE',  ( -73.25000000204839523, 65.69163855873948421, -25.81189881250000084 ) ) ;
#3805 = B_SPLINE_CURVE_WITH_KNOTS ( 'NONE', 3,
 ( #9264, #2014, #8435, #7490, #3643, #8200, #11112, #4721, #3758, #2750, #155, #3585, #8257, #8375, #6529, #6408, #9327, #2804, #2926, #7311, #10040, #6468, #11053, #1117, #9093, #6355, #2861, #7427, #33, #5446, #1834, #9984, #9151, #10097 ),
 .UNSPECIFIED., .F., .F.,
 ( 4, 2, 2, 2, 2, 2, 2, 2, 2, 2, 2, 2, 2, 2, 2, 2, 4 ),
 ( 0.02428132876980577601, 0.02579896738251766936, 0.02731660599522955923, 0.02807542530158549723, 0.02883424460794143523, 0.03035188322065331470, 0.03186952183336519417, 0.03338716044607706324, 0.03642243767150082911, 0.03794007628421271205, 0.03945771489692460193, 0.04021653420328053646, 0.04097535350963647099, 0.04249299212234831924, 0.04401063073506016055, 0.04552826934777200879, 0.04856354657319568446 ),
 .UNSPECIFIED. ) ;
#3806 = CARTESIAN_POINT ( 'NONE',  ( 0.8520517685207298353, 50.51279070969081175, -2.211769638084826184 ) ) ;
#3807 = EDGE_CURVE ( 'NONE', #7121, #3322, #8159, .T. ) ;
#3808 = CARTESIAN_POINT ( 'NONE',  ( 4.329456757236127551, 33.97246960341611555, -0.0004353087921988608999 ) ) ;
#3809 = ORIENTED_EDGE ( 'NONE', *, *, #485, .T. ) ;
#3810 = ADVANCED_FACE ( 'NONE', ( #9011 ), #6069, .F. ) ;
#3811 = CARTESIAN_POINT ( 'NONE',  ( -54.40418125752137968, 71.24517320114661345, 13.33400169942066249 ) ) ;
#3812 = EDGE_CURVE ( 'NONE', #4662, #723, #4524, .T. ) ;
#3813 = VECTOR ( 'NONE', #2769, 1000.000000000000000 ) ;
#3814 = CARTESIAN_POINT ( 'NONE',  ( 22.66666666666666785, 68.99999999999998579, 0.000000000000000000 ) ) ;
#3815 = DIRECTION ( 'NONE',  ( -1.000000000000000000, 0.000000000000000000, 0.000000000000000000 ) ) ;
#3816 = DIRECTION ( 'NONE',  ( -1.000000000000000000, -0.000000000000000000, -0.000000000000000000 ) ) ;
#3817 = CARTESIAN_POINT ( 'NONE',  ( -72.40625000000007105, 65.35533905932732068, -24.99999999999987921 ) ) ;
#3818 = ORIENTED_EDGE ( 'NONE', *, *, #3807, .T. ) ;
#3819 = CARTESIAN_POINT ( 'NONE',  ( -80.00000000000000000, 55.00000000000000000, -24.99999999999999645 ) ) ;
#3820 = CARTESIAN_POINT ( 'NONE',  ( -49.57393269579290518, 54.98425279022231393, 0.004738408210547216323 ) ) ;
#3821 = CARTESIAN_POINT ( 'NONE',  ( -61.54402485781515963, 52.35750010887923622, 4.247823058339725399 ) ) ;
#3822 = ADVANCED_FACE ( 'NONE', ( #2831 ), #7339, .F. ) ;
#3823 = ADVANCED_FACE ( 'NONE', ( #1987 ), #9067, .T. ) ;
#3824 = CIRCLE ( 'NONE', #936, 29.00000000000000355 ) ;
#3825 = CARTESIAN_POINT ( 'NONE',  ( -77.46875000000005684, 30.00000000000010303, 10.35533905932735443 ) ) ;
#3826 = AXIS2_PLACEMENT_3D ( 'NONE', #6130, #6072, #11552 ) ;
#3827 = EDGE_CURVE ( 'NONE', #2054, #10529, #4227, .T. ) ;
#3828 = DIRECTION ( 'NONE',  ( -0.000000000000000000, -0.000000000000000000, -1.000000000000000000 ) ) ;
#3829 = CARTESIAN_POINT ( 'NONE',  ( 16.10999105973513679, 58.51886257568109784, 6.100589661946206554 ) ) ;
#3830 = VERTEX_POINT ( 'NONE', #11380 ) ;
#3831 = CARTESIAN_POINT ( 'NONE',  ( 8.058385817489730485, 34.79396711235183659, 6.140502173211014103 ) ) ;
#3832 = UNCERTAINTY_MEASURE_WITH_UNIT (LENGTH_MEASURE( 1.000000000000000082E-05 ), #11105, 'distance_accuracy_value', 'NONE');
#3833 = CARTESIAN_POINT ( 'NONE',  ( 0.000000000000000000, 110.0000000000000000, 0.000000000000000000 ) ) ;
#3834 = DIRECTION ( 'NONE',  ( 0.000000000000000000, 1.000000000000000000, 0.000000000000000000 ) ) ;
#3835 = DIRECTION ( 'NONE',  ( -1.000000000000000000, 0.000000000000000000, 0.000000000000000000 ) ) ;
#3836 = CARTESIAN_POINT ( 'NONE',  ( -73.43750000204839523, 65.69163855873948421, -25.81189881250000440 ) ) ;
#3837 = CARTESIAN_POINT ( 'NONE',  ( -74.09375000204839523, 36.74823131438026280, 18.25176868561974786 ) ) ;
#3838 = ORIENTED_EDGE ( 'NONE', *, *, #6586, .F. ) ;
#3839 = CARTESIAN_POINT ( 'NONE',  ( -75.87500000204839523, 80.81189881250001861, 10.69163855873948599 ) ) ;
#3840 = EDGE_LOOP ( 'NONE', ( #3803, #4533, #10596 ) ) ;
#3841 = CARTESIAN_POINT ( 'NONE',  ( -31.83648591676323392, 41.19787054414934602, -2.739720031503523945 ) ) ;
#3842 = PLANE ( 'NONE',  #10150 ) ;
#3843 = DIRECTION ( 'NONE',  ( -1.000000000000000000, -0.000000000000000000, -0.000000000000000000 ) ) ;
#3844 = AXIS2_PLACEMENT_3D ( 'NONE', #2489, #1757, #8119 ) ;
#3845 = DIRECTION ( 'NONE',  ( 1.000000000000000000, 0.000000000000000000, 0.000000000000000000 ) ) ;
#3846 = ORIENTED_EDGE ( 'NONE', *, *, #3812, .T. ) ;
#3847 = AXIS2_PLACEMENT_3D ( 'NONE', #3185, #10483, #2285 ) ;
#3848 = AXIS2_PLACEMENT_3D ( 'NONE', #4753, #247, #6800 ) ;
#3849 = CARTESIAN_POINT ( 'NONE',  ( 0.000000000000000000, 0.000000000000000000, -3.996153373752295401 ) ) ;
#3850 = DIRECTION ( 'NONE',  ( -1.000000000000000000, -0.000000000000000000, -0.000000000000000000 ) ) ;
#3851 = CARTESIAN_POINT ( 'NONE',  ( -35.32265116553373474, 50.16047822658878630, -1.298113203157589934 ) ) ;
#3852 = FACE_OUTER_BOUND ( 'NONE', #11050, .T. ) ;
#3853 = CARTESIAN_POINT ( 'NONE',  ( -8.166495697937584453, 60.85006410611888583, -3.912655936626574071 ) ) ;
#3854 = CARTESIAN_POINT ( 'NONE',  ( -5.682122240792035761, 66.13352472168112683, 18.97764918900208997 ) ) ;
#3855 = CIRCLE ( 'NONE', #1366, 1.500000000000001332 ) ;
#3856 = AXIS2_PLACEMENT_3D ( 'NONE', #9987, #5566, #1727 ) ;
#3857 = DIRECTION ( 'NONE',  ( 0.000000000000000000, 0.000000000000000000, 1.000000000000000000 ) ) ;
#3858 = EDGE_LOOP ( 'NONE', ( #10295, #5561, #8934 ) ) ;
#3859 = CARTESIAN_POINT ( 'NONE',  ( -5.000000000000000000, -0.4878135028931869788, -6.100000000000001421 ) ) ;
#3860 = CARTESIAN_POINT ( 'NONE',  ( -2.500000000000003553, 4.330127018922192761, -6.099999999999999645 ) ) ;
#3861 = VERTEX_POINT ( 'NONE', #8470 ) ;
#3862 = EDGE_CURVE ( 'NONE', #3293, #9431, #1145, .T. ) ;
#3863 = CARTESIAN_POINT ( 'NONE',  ( 17.52230480588388417, 67.92092721363508190, 16.80419350660125843 ) ) ;
#3864 =( BOUNDED_SURFACE ( )  B_SPLINE_SURFACE ( 1, 2, ( 
 ( #3819, #4719, #6772, #2253, #1115, #275, #8373, #6590, #5866, #9505, #1233, #11350, #8496, #7488, #4963, #6712, #6825, #3882, #219, #1178, #3157, #10452, #11110, #9262, #3041, #9384, #11165, #7660, #397, #4902, #11293, #4845, #3106, #10220, #3938, #4000, #1297, #4779, #8618, #4065, #11231, #2924, #2012, #335, #9325, #10397, #8554, #7722, #8433, #7601, #2981, #6647, #2075, #5749, #10341, #2140, #5810, #5083, #8849, #9568, #7772, #3330, #510, #9682, #1361, #627, #4291, #5028, #8787, #9795, #11584, #8674, #568, #6999, #4173, #5991, #11643, #456, #8903, #9625, #9734, #7833, #1420, #7949, #4113, #11464, #2316, #685, #10571 ),
 ( #10622, #3387, #11402, #3272, #4358, #7062, #1532, #10512, #10686, #8728, #7894, #6103, #2497, #6945, #2372, #6045, #11524, #8009, #5256, #1477, #3452, #3215, #7122, #2434, #5138, #4236, #6162, #10745, #5198, #1588, #5925, #6883, #11708, #5428, #9133, #10973, #9911, #6447, #5546, #4527, #3737, #8295, #5484, #5313, #8239, #1814, #6392, #16, #855, #2611, #3685, #10021, #9189, #7175, #6337, #8183, #1707, #914, #6218, #4415, #11819, #9024, #9969, #9852, #4584, #7350, #1643, #9077, #10078, #2785, #8967, #3626, #7292, #801, #6280, #76, #742, #981, #5371, #1875, #4472, #8124, #4643, #8072, #11761, #10801, #7404, #7239, #10924 ) ),
 .UNSPECIFIED., .F., .F., .T. ) 
 B_SPLINE_SURFACE_WITH_KNOTS ( ( 2, 2 ),
 ( 3, 2, 2, 2, 2, 2, 2, 2, 2, 2, 2, 2, 2, 2, 2, 2, 2, 2, 2, 2, 2, 2, 2, 2, 2, 2, 2, 2, 2, 2, 2, 2, 2, 2, 2, 2, 2, 2, 2, 2, 2, 2, 2, 2, 3 ),
 ( 0.000000000000000000, 1.000000000000000000 ),
 ( 0.000000000000000000, 0.02083333333333333218, 0.04166666666666666435, 0.06250000000000000000, 0.08333333333333332871, 0.1041666666666666713, 0.1250000000000000000, 0.1458333333333333426, 0.1666666666666666574, 0.1875000000000000000, 0.2083333333333333426, 0.2291666666666666574, 0.2500000000000000000, 0.2708333333333333148, 0.2916666666666666852, 0.3125000000000000000, 0.3333333333333333148, 0.3541666666666666852, 0.3750000000000000000, 0.3958333333333333148, 0.4166666666666666852, 0.4375000000000000000, 0.4583333333333333148, 0.4791666666666666852, 0.5000000000000000000, 0.5208333333333333703, 0.5416666666666666297, 0.5625000000000000000, 0.5833333333333333703, 0.6041666666666666297, 0.6250000000000000000, 0.6458333333333333703, 0.6666666666666666297, 0.6875000000000000000, 0.7083333333333333703, 0.7291666666666666297, 0.7500000000000000000, 0.7708333333333333703, 0.7916666666666666297, 0.8125000000000000000, 0.8333333333333333703, 0.8541666666666666297, 0.8750000000000000000, 0.8888490471511721891, 0.8977375376226839343 ),
 .UNSPECIFIED. ) 
 GEOMETRIC_REPRESENTATION_ITEM ( )  RATIONAL_B_SPLINE_SURFACE ( (
 ( 1.000000000000000000, 0.9238795325112867385, 1.000000000000000000, 0.9238795325112867385, 1.000000000000000000, 0.9238795325112867385, 1.000000000000000000, 0.9238795325112867385, 1.000000000000000000, 0.9238795325112867385, 1.000000000000000000, 0.9238795325112867385, 1.000000000000000000, 0.9238795325112867385, 1.000000000000000000, 0.9238795325112867385, 1.000000000000000000, 0.9238795325112867385, 1.000000000000000000, 0.9238795325112867385, 1.000000000000000000, 0.9238795325112867385, 1.000000000000000000, 0.9238795325112867385, 1.000000000000000000, 0.9238795325112867385, 1.000000000000000000, 0.9238795325112867385, 1.000000000000000000, 0.9238795325112867385, 1.000000000000000000, 0.9238795325112867385, 1.000000000000000000, 0.9238795325112867385, 1.000000000000000000, 0.9238795325112867385, 1.000000000000000000, 0.9238795325112867385, 1.000000000000000000, 0.9238795325112867385, 1.000000000000000000, 0.9238795325112867385, 1.000000000000000000, 0.9238795325112867385, 1.000000000000000000, 0.9238795325112867385, 1.000000000000000000, 0.9238795325112867385, 1.000000000000000000, 0.9238795325112867385, 1.000000000000000000, 0.9238795325112867385, 1.000000000000000000, 0.9238795325112867385, 1.000000000000000000, 0.9238795325112867385, 1.000000000000000000, 0.9238795325112867385, 1.000000000000000000, 0.9238795325112867385, 1.000000000000000000, 0.9238795325112867385, 1.000000000000000000, 0.9238795325112867385, 1.000000000000000000, 0.9238795325112867385, 1.000000000000000000, 0.9238795325112867385, 1.000000000000000000, 0.9238795325112867385, 1.000000000000000000, 0.9238795325112867385, 1.000000000000000000, 0.9238795325112867385, 1.000000000000000000, 0.9238795325112867385, 1.000000000000000000, 0.9238795325112867385, 1.000000000000000000, 0.9238795325112867385, 1.000000000000000000, 0.9238795325112867385, 1.000000000000000000, 0.9238795325112867385, 1.000000000000000000, 0.9493985947158180005, 0.9660721892104719988, 0.9660721892104719988, 0.9660721892104719988),
 ( 1.000000000000000000, 0.9238795325112867385, 1.000000000000000000, 0.9238795325112867385, 1.000000000000000000, 0.9238795325112867385, 1.000000000000000000, 0.9238795325112867385, 1.000000000000000000, 0.9238795325112867385, 1.000000000000000000, 0.9238795325112867385, 1.000000000000000000, 0.9238795325112867385, 1.000000000000000000, 0.9238795325112867385, 1.000000000000000000, 0.9238795325112867385, 1.000000000000000000, 0.9238795325112867385, 1.000000000000000000, 0.9238795325112867385, 1.000000000000000000, 0.9238795325112867385, 1.000000000000000000, 0.9238795325112867385, 1.000000000000000000, 0.9238795325112867385, 1.000000000000000000, 0.9238795325112867385, 1.000000000000000000, 0.9238795325112867385, 1.000000000000000000, 0.9238795325112867385, 1.000000000000000000, 0.9238795325112867385, 1.000000000000000000, 0.9238795325112867385, 1.000000000000000000, 0.9238795325112867385, 1.000000000000000000, 0.9238795325112867385, 1.000000000000000000, 0.9238795325112867385, 1.000000000000000000, 0.9238795325112867385, 1.000000000000000000, 0.9238795325112867385, 1.000000000000000000, 0.9238795325112867385, 1.000000000000000000, 0.9238795325112867385, 1.000000000000000000, 0.9238795325112867385, 1.000000000000000000, 0.9238795325112867385, 1.000000000000000000, 0.9238795325112867385, 1.000000000000000000, 0.9238795325112867385, 1.000000000000000000, 0.9238795325112867385, 1.000000000000000000, 0.9238795325112867385, 1.000000000000000000, 0.9238795325112867385, 1.000000000000000000, 0.9238795325112867385, 1.000000000000000000, 0.9238795325112867385, 1.000000000000000000, 0.9238795325112867385, 1.000000000000000000, 0.9238795325112867385, 1.000000000000000000, 0.9238795325112867385, 1.000000000000000000, 0.9238795325112867385, 1.000000000000000000, 0.9238795325112867385, 1.000000000000000000, 0.9238795325112867385, 1.000000000000000000, 0.9238795325112867385, 1.000000000000000000, 0.9493985947158180005, 0.9660721892104719988, 0.9660721892104719988, 0.9660721892104719988) ) ) 
 REPRESENTATION_ITEM ( '' )  SURFACE ( )  );
#3865 = CARTESIAN_POINT ( 'NONE',  ( -73.06250000204840944, 80.81189881250001861, 10.69163855873948599 ) ) ;
#3866 = AXIS2_PLACEMENT_3D ( 'NONE', #2417, #4278, #6870 ) ;
#3867 = CARTESIAN_POINT ( 'NONE',  ( -80.00000000000001421, 54.99999999999999289, -16.97055937655931501 ) ) ;
#3868 = CARTESIAN_POINT ( 'NONE',  ( -48.85567157503042779, 75.97628680226326026, -2.745941867523475466 ) ) ;
#3869 = SURFACE_SIDE_STYLE ('',( #8418 ) ) ;
#3870 = CARTESIAN_POINT ( 'NONE',  ( -54.32961274566940801, 69.86573439484330095, 14.86481071665870601 ) ) ;
#3871 = EDGE_LOOP ( 'NONE', ( #1167, #1972, #3504, #375 ) ) ;
#3872 = CARTESIAN_POINT ( 'NONE',  ( 47.00000000000000711, 51.46446609406725514, 3.535533905932731091 ) ) ;
#3873 = DIRECTION ( 'NONE',  ( 0.000000000000000000, 0.000000000000000000, 1.000000000000000000 ) ) ;
#3874 = VERTEX_POINT ( 'NONE', #9356 ) ;
#3875 = CARTESIAN_POINT ( 'NONE',  ( -56.72452039520490530, 64.93179437211591676, 18.59801390061586801 ) ) ;
#3876 = CARTESIAN_POINT ( 'NONE',  ( -62.45014759628331547, 49.89181376149021219, 20.39015500988638507 ) ) ;
#3877 = FILL_AREA_STYLE ('',( #213 ) ) ;
#3878 = DIRECTION ( 'NONE',  ( -1.000000000000000000, -0.000000000000000000, -0.000000000000000000 ) ) ;
#3879 = CARTESIAN_POINT ( 'NONE',  ( -75.00000000000000000, 55.00000000000000000, 0.000000000000000000 ) ) ;
#3880 = CARTESIAN_POINT ( 'NONE',  ( -72.21875000000008527, 79.99999999999988631, -10.35533905932732601 ) ) ;
#3881 = VERTEX_POINT ( 'NONE', #4815 ) ;
#3882 = CARTESIAN_POINT ( 'NONE',  ( -78.40625000000000000, 65.35533905932737753, -24.99999999999999645 ) ) ;
#3883 = CARTESIAN_POINT ( 'NONE',  ( -24.09713505895794228, 55.00123344345425380, -0.01226757850090470087 ) ) ;
#3884 = DIRECTION ( 'NONE',  ( 0.8660254037844382635, 0.5000000000000004441, 0.000000000000000000 ) ) ;
#3885 = DIRECTION ( 'NONE',  ( -0.04756514941544910668, 0.9988681377244376103, -0.000000000000000000 ) ) ;
#3886 = DIRECTION ( 'NONE',  ( 0.000000000000000000, 1.000000000000000000, 0.000000000000000000 ) ) ;
#3887 = CARTESIAN_POINT ( 'NONE',  ( -61.03686256008624866, 55.68802913392543275, 13.99442384959076691 ) ) ;
#3888 = EDGE_LOOP ( 'NONE', ( #6818, #10413 ) ) ;
#3889 = CARTESIAN_POINT ( 'NONE',  ( 7.506399388638331338, 34.30832474160909129, 4.109400874309620200 ) ) ;
#3890 = CARTESIAN_POINT ( 'NONE',  ( 0.000000000000000000, 50.52094453300079380, 0.000000000000000000 ) ) ;
#3891 = EDGE_CURVE ( 'NONE', #10599, #3494, #5382, .T. ) ;
#3892 = DIRECTION ( 'NONE',  ( 1.000000000000000000, 0.000000000000000000, 0.000000000000000000 ) ) ;
#3893 = CARTESIAN_POINT ( 'NONE',  ( 3.000000000000000000, 3.673940397442059868E-16, -0.8895714285714284575 ) ) ;
#3894 = CARTESIAN_POINT ( 'NONE',  ( -5.866463102745652414, 66.55608005278446626, -22.17084374085253629 ) ) ;
#3895 = CARTESIAN_POINT ( 'NONE',  ( -72.68750000204839523, 44.30836144126053000, 25.81189881250000795 ) ) ;
#3896 = ORIENTED_EDGE ( 'NONE', *, *, #2216, .T. ) ;
#3897 = CARTESIAN_POINT ( 'NONE',  ( -72.40625000204839523, 36.74823131438026280, 18.25176868561974786 ) ) ;
#3898 = ORIENTED_EDGE ( 'NONE', *, *, #798, .F. ) ;
#3899 = CARTESIAN_POINT ( 'NONE',  ( 21.59285841830472918, 76.88861624364108138, -12.08424295940928772 ) ) ;
#3900 = CARTESIAN_POINT ( 'NONE',  ( 25.00000000000000000, 76.00000000000000000, 0.000000000000000000 ) ) ;
#3901 = EDGE_CURVE ( 'NONE', #3923, #1322, #8069, .T. ) ;
#3902 = DIRECTION ( 'NONE',  ( -0.000000000000000000, -0.000000000000000000, 1.000000000000000000 ) ) ;
#3903 = DIRECTION ( 'NONE',  ( 0.000000000000000000, 1.000000000000000000, 0.000000000000000000 ) ) ;
#3904 = DIRECTION ( 'NONE',  ( 1.000000000000000000, 6.033820786006286457E-17, -0.000000000000000000 ) ) ;
#3905 = ORIENTED_EDGE ( 'NONE', *, *, #2436, .F. ) ;
#3906 = CARTESIAN_POINT ( 'NONE',  ( -79.62500000000000000, 80.00000000000000000, -1.530808498934191324E-15 ) ) ;
#3907 = CARTESIAN_POINT ( 'NONE',  ( -73.25000000409677625, 30.00000000000000355, 4.592425496802573578E-15 ) ) ;
#3908 = DIRECTION ( 'NONE',  ( -1.000000000000000000, -0.000000000000000000, -0.000000000000000000 ) ) ;
#3909 = FACE_BOUND ( 'NONE', #4530, .T. ) ;
#3910 = CARTESIAN_POINT ( 'NONE',  ( -19.83316236458889747, 56.37610012593751208, 6.902063095245181579 ) ) ;
#3911 = DIRECTION ( 'NONE',  ( -1.000000000000000000, 0.000000000000000000, 0.000000000000000000 ) ) ;
#3912 = DIRECTION ( 'NONE',  ( -1.000000000000000000, 0.000000000000000000, 0.000000000000000000 ) ) ;
#3913 = ORIENTED_EDGE ( 'NONE', *, *, #6177, .T. ) ;
#3914 = DIRECTION ( 'NONE',  ( 0.000000000000000000, 0.000000000000000000, -1.000000000000000000 ) ) ;
#3915 = LINE ( 'NONE', #7523, #8630 ) ;
#3916 = ORIENTED_EDGE ( 'NONE', *, *, #6143, .F. ) ;
#3917 = EDGE_CURVE ( 'NONE', #3830, #10858, #630, .T. ) ;
#3918 = CARTESIAN_POINT ( 'NONE',  ( -62.45014759628331547, 49.89181376149021219, 20.39015500988638507 ) ) ;
#3919 = CARTESIAN_POINT ( 'NONE',  ( -75.59375000204839523, 55.00000000000000000, 25.81189881249999729 ) ) ;
#3920 = CARTESIAN_POINT ( 'NONE',  ( -80.00000000000001421, 71.97056274847716395, 1.500003371917795425 ) ) ;
#3921 = CARTESIAN_POINT ( 'NONE',  ( 34.00000000000000000, 64.99999999999998579, 0.000000000000000000 ) ) ;
#3922 = DIRECTION ( 'NONE',  ( 1.000000000000000000, 6.033820786006286457E-17, 0.000000000000000000 ) ) ;
#3923 = VERTEX_POINT ( 'NONE', #4088 ) ;
#3924 = DIRECTION ( 'NONE',  ( 1.000000000000000000, 0.000000000000000000, 0.000000000000000000 ) ) ;
#3925 = CARTESIAN_POINT ( 'NONE',  ( -72.21875000409676204, 65.35533905932712173, 25.00000000000025580 ) ) ;
#3926 = VECTOR ( 'NONE', #10850, 1000.000000000000000 ) ;
#3927 = DIRECTION ( 'NONE',  ( 0.000000000000000000, 1.000000000000000000, 0.000000000000000000 ) ) ;
#3928 = PRESENTATION_LAYER_ASSIGNMENT (  '', '', ( #4316 ) ) ;
#3929 = EDGE_LOOP ( 'NONE', ( #1758, #3898 ) ) ;
#3930 = CARTESIAN_POINT ( 'NONE',  ( -61.11681434411291036, 49.89209620109770071, 20.38939785324081200 ) ) ;
#3931 = CARTESIAN_POINT ( 'NONE',  ( 3.998131555863420505, 40.98098423833228310, -0.0003514993523973195672 ) ) ;
#3932 = DIRECTION ( 'NONE',  ( 0.000000000000000000, 1.000000000000000000, 0.000000000000000000 ) ) ;
#3933 = CARTESIAN_POINT ( 'NONE',  ( -76.25000000409677625, 30.00000000000000355, 4.592425496802573578E-15 ) ) ;
#3934 = EDGE_CURVE ( 'NONE', #3307, #11779, #9022, .T. ) ;
#3935 = CARTESIAN_POINT ( 'NONE',  ( -78.00000000000002842, 42.27207793864211283, -4.242637315201479353 ) ) ;
#3936 = DIRECTION ( 'NONE',  ( 1.000000000000000000, 6.033820786006286457E-17, -0.000000000000000000 ) ) ;
#3937 = EDGE_LOOP ( 'NONE', ( #6150, #4696, #10836, #4364 ) ) ;
#3938 = CARTESIAN_POINT ( 'NONE',  ( -76.81250000000000000, 72.67766952966368876, -17.67766952966368876 ) ) ;
#3939 = CARTESIAN_POINT ( 'NONE',  ( -78.00000000000002842, 46.51471862576140381, 8.485284746156354529 ) ) ;
#3940 = FACE_OUTER_BOUND ( 'NONE', #9972, .T. ) ;
#3941 = CIRCLE ( 'NONE', #10620, 2.500000000000000000 ) ;
#3942 = CARTESIAN_POINT ( 'NONE',  ( -75.12500000409677625, 55.00000000000000000, 24.99999999999999645 ) ) ;
#3943 = CARTESIAN_POINT ( 'NONE',  ( 11.44321751246060437, 53.17432586545520223, 6.801933848413093564 ) ) ;
#3944 = ORIENTED_EDGE ( 'NONE', *, *, #1308, .F. ) ;
#3945 = CARTESIAN_POINT ( 'NONE',  ( 21.85574933723554736, 73.37275400661043534, 10.58193396047185075 ) ) ;
#3946 = CIRCLE ( 'NONE', #2797, 1.500000000000001332 ) ;
#3947 = CARTESIAN_POINT ( 'NONE',  ( 36.99999999999999289, 55.00000000000000000, -22.00000000000000000 ) ) ;
#3948 = ADVANCED_FACE ( 'NONE', ( #6743 ), #201, .F. ) ;
#3949 = FACE_OUTER_BOUND ( 'NONE', #6340, .T. ) ;
#3950 = DIRECTION ( 'NONE',  ( 0.000000000000000000, 1.000000000000000000, 0.000000000000000000 ) ) ;
#3951 = CARTESIAN_POINT ( 'NONE',  ( -24.49417083054724742, 79.31944638913208223, 5.853031391697339991 ) ) ;
#3952 = CARTESIAN_POINT ( 'NONE',  ( -71.84375000204838102, 73.25176868561975141, -18.25176868561974430 ) ) ;
#3953 = AXIS2_PLACEMENT_3D ( 'NONE', #1522, #7052, #8839 ) ;
#3954 = VERTEX_POINT ( 'NONE', #4936 ) ;
#3955 = CARTESIAN_POINT ( 'NONE',  ( -72.78125000204839523, 73.25176868561975141, 18.25176868561974075 ) ) ;
#3956 = ORIENTED_EDGE ( 'NONE', *, *, #5685, .F. ) ;
#3957 = CARTESIAN_POINT ( 'NONE',  ( 25.18797318253816186, 79.91260864020590304, -2.131801228107524704 ) ) ;
#3958 = CARTESIAN_POINT ( 'NONE',  ( -68.00371502632826548, 40.99428914066987062, 0.003597212120264942775 ) ) ;
#3959 = AXIS2_PLACEMENT_3D ( 'NONE', #1976, #7510, #9229 ) ;
#3960 = EDGE_CURVE ( 'NONE', #4962, #4282, #10427, .T. ) ;
#3961 = DIRECTION ( 'NONE',  ( -1.000000000000000000, 0.000000000000000000, 0.000000000000000000 ) ) ;
#3962 = FACE_OUTER_BOUND ( 'NONE', #3871, .T. ) ;
#3963 = CARTESIAN_POINT ( 'NONE',  ( -75.50000000000001421, 54.99999999999944578, -24.99999999999999645 ) ) ;
#3964 = ADVANCED_FACE ( 'NONE', ( #4034 ), #11103, .T. ) ;
#3965 = VERTEX_POINT ( 'NONE', #1334 ) ;
#3966 = ADVANCED_FACE ( 'NONE', ( #4997 ), #2314, .T. ) ;
#3967 = CARTESIAN_POINT ( 'NONE',  ( -77.75000000000000000, 55.00000000000000000, 24.99999999999999645 ) ) ;
#3968 = CARTESIAN_POINT ( 'NONE',  ( -72.31250000409677625, 72.67766952966368876, 17.67766952966368521 ) ) ;
#3969 = CONICAL_SURFACE ( 'NONE', #1083, 5.000000000000000888, 1.047197551196596299 ) ;
#3970 = CARTESIAN_POINT ( 'NONE',  ( -43.48657495774332915, 55.33066324073525521, -4.991758028738959574 ) ) ;
#3971 = ORIENTED_EDGE ( 'NONE', *, *, #11621, .F. ) ;
#3972 = CARTESIAN_POINT ( 'NONE',  ( 1.556783352007605314, 50.68022262062438443, -5.615603207694791266 ) ) ;
#3973 = CARTESIAN_POINT ( 'NONE',  ( -72.68750000000007105, 37.32233047033641071, -17.67766952966357863 ) ) ;
#3974 = AXIS2_PLACEMENT_3D ( 'NONE', #11143, #9243, #2172 ) ;
#3975 = DIRECTION ( 'NONE',  ( -1.000000000000000000, -6.033820786006286457E-17, -0.000000000000000000 ) ) ;
#3976 = ADVANCED_FACE ( 'NONE', ( #10721 ), #2532, .T. ) ;
#3977 = ORIENTED_EDGE ( 'NONE', *, *, #3301, .T. ) ;
#3978 = CARTESIAN_POINT ( 'NONE',  ( -5.000000000000000000, -2.886751345948134428, -5.653418012614792154 ) ) ;
#3979 = CARTESIAN_POINT ( 'NONE',  ( -79.25000000204839523, 80.81189881250000440, -10.69163855873948954 ) ) ;
#3980 = ORIENTED_EDGE ( 'NONE', *, *, #2392, .T. ) ;
#3981 = CARTESIAN_POINT ( 'NONE',  ( -42.03064326886630653, 53.96872019721284630, -20.99365203016559178 ) ) ;
#3982 = CARTESIAN_POINT ( 'NONE',  ( -74.75000000204840944, 65.69163855873948421, -25.81189881250000440 ) ) ;
#3983 = CARTESIAN_POINT ( 'NONE',  ( 39.99999999999999289, 55.00000000000000000, 0.000000000000000000 ) ) ;
#3984 = CARTESIAN_POINT ( 'NONE',  ( -59.00490307935969270, 55.00061426705308065, 21.02882928537637497 ) ) ;
#3985 =( NAMED_UNIT ( * ) SI_UNIT ( $, .STERADIAN. ) SOLID_ANGLE_UNIT ( ) );
#3986 = CARTESIAN_POINT ( 'NONE',  ( -77.56250000409679046, 37.32233047033631124, -17.67766952966368166 ) ) ;
#3987 = VERTEX_POINT ( 'NONE', #9771 ) ;
#3988 = CARTESIAN_POINT ( 'NONE',  ( 14.99999999999999645, 39.99999999999999289, -20.00000000000000000 ) ) ;
#3989 = CARTESIAN_POINT ( 'NONE',  ( 2.790000683316907093, 50.03283139526183732, -0.6581345825051299059 ) ) ;
#3990 = CARTESIAN_POINT ( 'NONE',  ( 12.14423903554155793, 49.50741477678717928, 20.43476828740966766 ) ) ;
#3991 = ORIENTED_EDGE ( 'NONE', *, *, #5968, .T. ) ;
#3992 = CARTESIAN_POINT ( 'NONE',  ( 10.47760422355487897, 42.10669920038468206, 16.77626177829396426 ) ) ;
#3993 = CARTESIAN_POINT ( 'NONE',  ( 17.20616264586559652, 63.61741959817585013, 11.20704532413626708 ) ) ;
#3994 = CARTESIAN_POINT ( 'NONE',  ( -79.15625000000001421, 44.64466094067263668, 24.99999999999997513 ) ) ;
#3995 = DIRECTION ( 'NONE',  ( 0.000000000000000000, 1.000000000000000000, 0.000000000000000000 ) ) ;
#3996 = UNCERTAINTY_MEASURE_WITH_UNIT (LENGTH_MEASURE( 1.000000000000000082E-05 ), #1998, 'distance_accuracy_value', 'NONE');
#3997 = CYLINDRICAL_SURFACE ( 'NONE', #6900, 1.500000000000000000 ) ;
#3998 = CIRCLE ( 'NONE', #3060, 2.500000000000000000 ) ;
#3999 = EDGE_LOOP ( 'NONE', ( #5040, #9297, #7167, #3538, #5019, #7487, #414, #1370 ) ) ;
#4000 = CARTESIAN_POINT ( 'NONE',  ( -76.71875000000000000, 80.00000000000001421, -10.35533905932737753 ) ) ;
#4001 = CARTESIAN_POINT ( 'NONE',  ( -78.87500000409677625, 55.00000000000000000, -24.99999999999999645 ) ) ;
#4002 = FILL_AREA_STYLE ('',( #337 ) ) ;
#4003 = CIRCLE ( 'NONE', #2851, 2.500000000000000000 ) ;
#4004 = CARTESIAN_POINT ( 'NONE',  ( 53.00000000000000000, 55.00000000000000000, -6.000000000000000000 ) ) ;
#4005 = CARTESIAN_POINT ( 'NONE',  ( -7.999860312172237364, 57.68304994702459254, -6.476756063187334433 ) ) ;
#4006 = CIRCLE ( 'NONE', #4774, 2.500000000000000000 ) ;
#4007 = ORIENTED_EDGE ( 'NONE', *, *, #3608, .F. ) ;
#4008 = CARTESIAN_POINT ( 'NONE',  ( -41.78535879711923684, 60.10680040617825881, -20.39053309953287751 ) ) ;
#4009 = DIRECTION ( 'NONE',  ( 0.000000000000000000, 0.000000000000000000, -1.000000000000000000 ) ) ;
#4010 = CARTESIAN_POINT ( 'NONE',  ( -2.500000000000000000, 3.061616997868383141E-16, -4.696360911962001339 ) ) ;
#4011 = LINE ( 'NONE', #2810, #10644 ) ;
#4012 = EDGE_CURVE ( 'NONE', #5247, #1715, #3094, .T. ) ;
#4013 = CARTESIAN_POINT ( 'NONE',  ( 2.500000000000000000, 0.000000000000000000, -6.099999999999999645 ) ) ;
#4014 = CARTESIAN_POINT ( 'NONE',  ( -74.46875000204839523, 73.25176868561975141, 18.25176868561974075 ) ) ;
#4015 = ORIENTED_EDGE ( 'NONE', *, *, #48, .F. ) ;
#4016 = CARTESIAN_POINT ( 'NONE',  ( -77.37500000409677625, 55.00000000000000000, -24.99999999999999645 ) ) ;
#4017 = EDGE_LOOP ( 'NONE', ( #6701, #509, #9041, #4807 ) ) ;
#4018 = CARTESIAN_POINT ( 'NONE',  ( -80.00000000000001421, 59.24264068711928388, -12.72791868944003824 ) ) ;
#4019 = CIRCLE ( 'NONE', #5543, 1.500000000000001332 ) ;
#4020 = CARTESIAN_POINT ( 'NONE',  ( -38.83024551010986869, 52.26031083538927646, -13.79250609426764385 ) ) ;
#4021 = CARTESIAN_POINT ( 'NONE',  ( 4.171999999999999709, -17.00000000000000000, 0.000000000000000000 ) ) ;
#4022 = CARTESIAN_POINT ( 'NONE',  ( 4.999999999999998224, -2.886751345948137981, -5.653418012614792154 ) ) ;
#4023 = PLANE ( 'NONE',  #6481 ) ;
#4024 = EDGE_CURVE ( 'NONE', #9967, #2595, #2657, .T. ) ;
#4025 = AXIS2_PLACEMENT_3D ( 'NONE', #9147, #994, #2566 ) ;
#4026 = ORIENTED_EDGE ( 'NONE', *, *, #6036, .F. ) ;
#4027 = CARTESIAN_POINT ( 'NONE',  ( -77.84375000000001421, 65.35533905932737753, 24.99999999999999645 ) ) ;
#4028 = CARTESIAN_POINT ( 'NONE',  ( -71.56250000409677625, 37.32233047033631124, -17.67766952966368166 ) ) ;
#4029 = CARTESIAN_POINT ( 'NONE',  ( -38.04614405021798262, 51.23507084643394194, -3.306421959314382875 ) ) ;
#4030 = ORIENTED_EDGE ( 'NONE', *, *, #8000, .T. ) ;
#4031 = CARTESIAN_POINT ( 'NONE',  ( -4.375366960226389601, 57.35780173001101900, -6.590899248362319440 ) ) ;
#4032 = PRODUCT_DEFINITION ( 'UNKNOWN', '', #9471, #10598 ) ;
#4033 = VECTOR ( 'NONE', #2113, 1000.000000000000000 ) ;
#4034 = FACE_OUTER_BOUND ( 'NONE', #189, .T. ) ;
#4035 = DIRECTION ( 'NONE',  ( -0.8191520442889974607, 0.000000000000000000, -0.5735764363510379438 ) ) ;
#4036 = EDGE_LOOP ( 'NONE', ( #9975, #8707 ) ) ;
#4037 = DIRECTION ( 'NONE',  ( 1.000000000000000000, 0.000000000000000000, 0.000000000000000000 ) ) ;
#4038 = CIRCLE ( 'NONE', #8241, 1.500000000000001332 ) ;
#4039 = DIRECTION ( 'NONE',  ( 0.000000000000000000, 1.000000000000000000, 0.000000000000000000 ) ) ;
#4040 = VERTEX_POINT ( 'NONE', #8043 ) ;
#4041 = CARTESIAN_POINT ( 'NONE',  ( -64.51030549024622474, 43.28227691760346119, 17.55408017169854418 ) ) ;
#4042 = CIRCLE ( 'NONE', #1925, 3.000000000000000000 ) ;
#4043 = CARTESIAN_POINT ( 'NONE',  ( -73.25000000204839523, 65.69163855873948421, -25.81189881250000440 ) ) ;
#4044 = EDGE_CURVE ( 'NONE', #7325, #1879, #6924, .T. ) ;
#4045 = FACE_OUTER_BOUND ( 'NONE', #6490, .T. ) ;
#4046 = CARTESIAN_POINT ( 'NONE',  ( -60.45014771802851072, 49.89223742090062075, 20.38901927491476584 ) ) ;
#4047 = VECTOR ( 'NONE', #3908, 1000.000000000000000 ) ;
#4048 = CIRCLE ( 'NONE', #10725, 4.999999999999990230 ) ;
#4049 = CARTESIAN_POINT ( 'NONE',  ( -77.75000000409677625, 30.00000000000000355, 4.592425496802573578E-15 ) ) ;
#4050 = ORIENTED_EDGE ( 'NONE', *, *, #4153, .F. ) ;
#4051 = EDGE_CURVE ( 'NONE', #6251, #52, #8441, .T. ) ;
#4052 = CARTESIAN_POINT ( 'NONE',  ( 0.000000000000000000, 0.000000000000000000, -6.099999999999999645 ) ) ;
#4053 = EDGE_CURVE ( 'NONE', #8475, #7495, #4314, .T. ) ;
#4054 = CARTESIAN_POINT ( 'NONE',  ( -1.443735181952766178, 4.939961795957295010, -0.08165819712376964912 ) ) ;
#4055 = CARTESIAN_POINT ( 'NONE',  ( -19.88142569839470042, 67.52672413929985851, 16.89011978890229315 ) ) ;
#4056 = ORIENTED_EDGE ( 'NONE', *, *, #8254, .F. ) ;
#4057 = AXIS2_PLACEMENT_3D ( 'NONE', #4487, #8138, #10819 ) ;
#4058 = CARTESIAN_POINT ( 'NONE',  ( -8.404080175971420985, 68.33445312550857409, -16.24552120034004332 ) ) ;
#4059 = CARTESIAN_POINT ( 'NONE',  ( -29.83024526348565431, 43.30463061081272969, 7.809786529886623363 ) ) ;
#4060 = AXIS2_PLACEMENT_3D ( 'NONE', #11748, #4512, #3554 ) ;
#4061 = DIRECTION ( 'NONE',  ( 0.000000000000000000, 1.000000000000000000, 0.000000000000000000 ) ) ;
#4062 = CARTESIAN_POINT ( 'NONE',  ( -76.15625000409677625, 30.00000000000000355, -10.35533905932738108 ) ) ;
#4063 = CARTESIAN_POINT ( 'NONE',  ( -1.734723475976807094E-14, -5.773502691896260863, -0.4465819873852071575 ) ) ;
#4064 = ORIENTED_EDGE ( 'NONE', *, *, #4089, .T. ) ;
#4065 = CARTESIAN_POINT ( 'NONE',  ( -76.34375000000001421, 65.35533905932737753, 24.99999999999999645 ) ) ;
#4066 = CARTESIAN_POINT ( 'NONE',  ( -74.99999999999998579, 39.36515909056227258, -20.53791299142420712 ) ) ;
#4067 = CARTESIAN_POINT ( 'NONE',  ( 52.99999999999999289, 55.00000000000000000, 0.000000000000000000 ) ) ;
#4068 = CARTESIAN_POINT ( 'NONE',  ( -33.95794589294774823, 47.99441920491325675, -0.3443687011034463619 ) ) ;
#4069 = ORIENTED_EDGE ( 'NONE', *, *, #1402, .F. ) ;
#4070 = CARTESIAN_POINT ( 'NONE',  ( -11.52239577449127061, 75.97627689174807131, -2.745668057393931161 ) ) ;
#4071 = CARTESIAN_POINT ( 'NONE',  ( -52.42856357389445066, 59.99999999999997158, -5.034386850915387018E-15 ) ) ;
#4072 = CARTESIAN_POINT ( 'NONE',  ( -78.00000000000001421, 54.99999999999999289, -18.47055937655931501 ) ) ;
#4073 = CARTESIAN_POINT ( 'NONE',  ( -75.03125000204839523, 36.74823131438024859, -18.25176868561973720 ) ) ;
#4074 = CARTESIAN_POINT ( 'NONE',  ( -25.19064713987262394, 79.91490204074258941, 2.105276644174951084 ) ) ;
#4075 = CARTESIAN_POINT ( 'NONE',  ( -78.31250000204839523, 29.18810118750000981, 10.69163855873950020 ) ) ;
#4076 = ORIENTED_EDGE ( 'NONE', *, *, #10279, .F. ) ;
#4077 = CARTESIAN_POINT ( 'NONE',  ( -77.75000000409677625, 30.00000000000000355, 4.592425496802573578E-15 ) ) ;
#4078 = CARTESIAN_POINT ( 'NONE',  ( 16.47760469315713294, 57.74566955740679930, 20.97627666568605420 ) ) ;
#4079 = CARTESIAN_POINT ( 'NONE',  ( -79.25000000204839523, 80.81189881250000440, -10.69163855873948954 ) ) ;
#4080 = CARTESIAN_POINT ( 'NONE',  ( 53.00000000000000000, 51.46446609406726935, 3.535533905932731091 ) ) ;
#4081 = CARTESIAN_POINT ( 'NONE',  ( 0.000000000000000000, 0.000000000000000000, 5.000000000000000000 ) ) ;
#4082 = ORIENTED_EDGE ( 'NONE', *, *, #6074, .F. ) ;
#4083 = CARTESIAN_POINT ( 'NONE',  ( -76.90625000000000000, 65.35533905932737753, -24.99999999999999645 ) ) ;
#4084 = CARTESIAN_POINT ( 'NONE',  ( -71.28125000409677625, 65.35533905932737753, -24.99999999999999645 ) ) ;
#4085 = CARTESIAN_POINT ( 'NONE',  ( -49.31852470631967122, 59.33770604155814254, -2.508136721262845370 ) ) ;
#4086 = ORIENTED_EDGE ( 'NONE', *, *, #4187, .F. ) ;
#4087 = CARTESIAN_POINT ( 'NONE',  ( 13.22345001879655335, 51.46496636567017191, 6.139952220504262037 ) ) ;
#4088 = CARTESIAN_POINT ( 'NONE',  ( 2.500000000000003109, -4.330127018922193649, 0.000000000000000000 ) ) ;
#4089 = EDGE_CURVE ( 'NONE', #3028, #9787, #4234, .T. ) ;
#4090 = CARTESIAN_POINT ( 'NONE',  ( 47.00000000000000000, 55.00000000000000000, 0.000000000000000000 ) ) ;
#4091 = ORIENTED_EDGE ( 'NONE', *, *, #298, .T. ) ;
#4092 = CARTESIAN_POINT ( 'NONE',  ( 15.85754866970926358, 72.28899002677383123, 13.64810891474729004 ) ) ;
#4093 = CARTESIAN_POINT ( 'NONE',  ( -1.443735181952766622, 4.939961795957295898, -6.018341802876231661 ) ) ;
#4094 = ORIENTED_EDGE ( 'NONE', *, *, #9085, .T. ) ;
#4095 = VECTOR ( 'NONE', #2329, 1000.000000000000000 ) ;
#4096 = APPLICATION_CONTEXT ( 'automotive_design' ) ;
#4097 = CARTESIAN_POINT ( 'NONE',  ( -72.50000000204839523, 44.30836144126053000, 25.81189881250000795 ) ) ;
#4098 = DIRECTION ( 'NONE',  ( -1.000000000000000000, -0.000000000000000000, -0.000000000000000000 ) ) ;
#4099 = CARTESIAN_POINT ( 'NONE',  ( -79.71875000000000000, 79.99999999999998579, -10.35533905932736332 ) ) ;
#4100 = LINE ( 'NONE', #6811, #874 ) ;
#4101 = EDGE_LOOP ( 'NONE', ( #4706, #11773, #10349, #3607 ) ) ;
#4102 = CARTESIAN_POINT ( 'NONE',  ( -78.00000000000002842, 38.02943725152282184, 3.371917797929946392E-06 ) ) ;
#4103 = EDGE_CURVE ( 'NONE', #9830, #1810, #5115, .T. ) ;
#4104 = CARTESIAN_POINT ( 'NONE',  ( -9.969360172258976860, 70.58303384883494402, -14.12411716821732277 ) ) ;
#4105 = ORIENTED_EDGE ( 'NONE', *, *, #5780, .F. ) ;
#4106 = CARTESIAN_POINT ( 'NONE',  ( -10.17314267936212069, 72.54319253558377056, -11.73149487979574168 ) ) ;
#4107 = CARTESIAN_POINT ( 'NONE',  ( -35.07137196547176927, 41.55265658068579171, -4.083739209675547599 ) ) ;
#4108 = DIRECTION ( 'NONE',  ( 0.000000000000000000, 1.000000000000000000, 0.000000000000000000 ) ) ;
#4109 = CARTESIAN_POINT ( 'NONE',  ( 36.99999999999999289, 50.00000000000001421, 6.123233995736750505E-16 ) ) ;
#4110 = CARTESIAN_POINT ( 'NONE',  ( -15.48546139901933572, 59.99999999999970157, 0.3308755477335553197 ) ) ;
#4111 = ADVANCED_FACE ( 'NONE', ( #5234, #6976 ), #2469, .T. ) ;
#4112 = ORIENTED_EDGE ( 'NONE', *, *, #1668, .F. ) ;
#4113 = CARTESIAN_POINT ( 'NONE',  ( -72.12500000000000000, 80.00000000000000000, -1.530808498934191324E-15 ) ) ;
#4114 = CARTESIAN_POINT ( 'NONE',  ( -75.00000000000002842, 40.04116987730228772, -21.05253787605388638 ) ) ;
#4115 = DIRECTION ( 'NONE',  ( 0.000000000000000000, 1.000000000000000000, 0.000000000000000000 ) ) ;
#4116 = DIRECTION ( 'NONE',  ( -1.000000000000000000, -0.000000000000000000, -0.000000000000000000 ) ) ;
#4117 = CARTESIAN_POINT ( 'NONE',  ( -45.33346893179080439, 57.68097894510658108, -6.473283064943208487 ) ) ;
#4118 = ORIENTED_EDGE ( 'NONE', *, *, #2922, .F. ) ;
#4119 = EDGE_CURVE ( 'NONE', #9864, #9375, #11484, .T. ) ;
#4120 = CARTESIAN_POINT ( 'NONE',  ( -39.16026728571524984, 50.89059911655681390, -20.69167526169209026 ) ) ;
#4121 = DIRECTION ( 'NONE',  ( 0.000000000000000000, 0.000000000000000000, -1.000000000000000000 ) ) ;
#4122 = CARTESIAN_POINT ( 'NONE',  ( 0.000000000000000000, -57.00000000000000000, -4.999999999999997335 ) ) ;
#4123 = CARTESIAN_POINT ( 'NONE',  ( -77.00000000204839523, 44.30836144126052289, 25.81189881250000795 ) ) ;
#4124 = CARTESIAN_POINT ( 'NONE',  ( -25.23647670057383152, 79.95418391132277236, -1.735782755942627542 ) ) ;
#4125 = CARTESIAN_POINT ( 'NONE',  ( -74.28125000204839523, 73.25176868561975141, 18.25176868561974075 ) ) ;
#4126 = ORIENTED_EDGE ( 'NONE', *, *, #8627, .F. ) ;
#4127 = CARTESIAN_POINT ( 'NONE',  ( -72.68750000409677625, 72.67766952966368876, -17.67766952966368876 ) ) ;
#4128 = PLANE ( 'NONE',  #2094 ) ;
#4129 = LINE ( 'NONE', #6786, #215 ) ;
#4130 = AXIS2_PLACEMENT_3D ( 'NONE', #3939, #2195, #7545 ) ;
#4131 = CARTESIAN_POINT ( 'NONE',  ( 0.1442708919848544047, 44.43605983923426805, -18.32883121229183487 ) ) ;
#4132 = DIRECTION ( 'NONE',  ( -0.000000000000000000, -0.000000000000000000, -1.000000000000000000 ) ) ;
#4133 = DIRECTION ( 'NONE',  ( 0.000000000000000000, 0.000000000000000000, 1.000000000000000000 ) ) ;
#4134 = CARTESIAN_POINT ( 'NONE',  ( -75.00000000000000000, 55.00000000000000000, 0.000000000000000000 ) ) ;
#4135 = EDGE_LOOP ( 'NONE', ( #7150, #7256, #5213, #3691 ) ) ;
#4136 = AXIS2_PLACEMENT_3D ( 'NONE', #8661, #3922, #9490 ) ;
#4137 = LINE ( 'NONE', #2279, #1828 ) ;
#4138 = CARTESIAN_POINT ( 'NONE',  ( -73.34375000000001421, 65.35533905932737753, 24.99999999999999645 ) ) ;
#4139 = CARTESIAN_POINT ( 'NONE',  ( 3.351853367131007122, -3.838309248099025961, -4.312635593573742646E-16 ) ) ;
#4140 = VECTOR ( 'NONE', #3749, 1000.000000000000000 ) ;
#4141 = CARTESIAN_POINT ( 'NONE',  ( -48.54021952654307626, 58.97499403197477363, -3.050551747025779914 ) ) ;
#4142 = ORIENTED_EDGE ( 'NONE', *, *, #1460, .F. ) ;
#4143 = CARTESIAN_POINT ( 'NONE',  ( -61.83316972777281961, 51.09090217642938114, 5.855680158205122332 ) ) ;
#4144 = CARTESIAN_POINT ( 'NONE',  ( -78.59375000409677625, 80.00000000000001421, -10.35533905932737753 ) ) ;
#4145 = CARTESIAN_POINT ( 'NONE',  ( -3.351853367131005346, 3.838309248099017523, -6.100000000000003197 ) ) ;
#4146 = ORIENTED_EDGE ( 'NONE', *, *, #10001, .F. ) ;
#4147 = CARTESIAN_POINT ( 'NONE',  ( 6.021660879821575385, 66.27766067927709059, -18.89023547443478179 ) ) ;
#4148 = AXIS2_PLACEMENT_3D ( 'NONE', #7916, #5830, #6905 ) ;
#4149 = CARTESIAN_POINT ( 'NONE',  ( -1.653121499799247163, 4.819072548984006943, -6.048595712916175593 ) ) ;
#4150 = AXIS2_PLACEMENT_3D ( 'NONE', #10387, #9313, #2968 ) ;
#4151 = ORIENTED_EDGE ( 'NONE', *, *, #11054, .T. ) ;
#4152 = CARTESIAN_POINT ( 'NONE',  ( -74.18750000204839523, 65.69163855873949842, 25.81189881250000440 ) ) ;
#4153 = EDGE_CURVE ( 'NONE', #7832, #6455, #1160, .T. ) ;
#4154 = DIRECTION ( 'NONE',  ( 1.000000000000000000, 0.000000000000000000, 0.000000000000000000 ) ) ;
#4155 = FACE_OUTER_BOUND ( 'NONE', #4323, .T. ) ;
#4156 = CARTESIAN_POINT ( 'NONE',  ( -14.23626113480177935, 55.01767704715457796, 0.008670778123901936099 ) ) ;
#4157 = CIRCLE ( 'NONE', #10455, 5.000000000000000000 ) ;
#4158 = CIRCLE ( 'NONE', #8574, 4.999999999999997335 ) ;
#4159 = DIRECTION ( 'NONE',  ( -0.000000000000000000, -0.000000000000000000, -1.000000000000000000 ) ) ;
#4160 = EDGE_LOOP ( 'NONE', ( #6165, #5954, #3510, #4606, #5896, #5396, #8610, #1534 ) ) ;
#4161 = CARTESIAN_POINT ( 'NONE',  ( -75.06471690751966719, 48.34131301757658150, 24.99999999999992184 ) ) ;
#4162 = EDGE_CURVE ( 'NONE', #8007, #4492, #5978, .T. ) ;
#4163 = CARTESIAN_POINT ( 'NONE',  ( -17.82693376281896391, 72.53768310958322729, 11.72612467905221934 ) ) ;
#4164 = VERTEX_POINT ( 'NONE', #1569 ) ;
#4165 = CARTESIAN_POINT ( 'NONE',  ( -62.30250798370089882, 46.00592899164083605, 19.01213062829916112 ) ) ;
#4166 = CARTESIAN_POINT ( 'NONE',  ( -21.07727389599352819, 61.60348718499724896, 12.35586511164976287 ) ) ;
#4167 = CARTESIAN_POINT ( 'NONE',  ( 2.500000000000000000, 0.000000000000000000, -3.832189483390572970 ) ) ;
#4168 = CARTESIAN_POINT ( 'NONE',  ( 2.500000000000005773, 4.330127018922190985, 0.000000000000000000 ) ) ;
#4169 = VECTOR ( 'NONE', #3237, 1000.000000000000114 ) ;
#4170 = CARTESIAN_POINT ( 'NONE',  ( -27.54087155171534462, 52.49442175028256230, 4.339376312279030756 ) ) ;
#4171 = ORIENTED_EDGE ( 'NONE', *, *, #6906, .T. ) ;
#4172 = SHAPE_REPRESENTATION ( 'Table Clamp Lock Screw', ( #4738 ), #844 ) ;
#4173 = CARTESIAN_POINT ( 'NONE',  ( -73.06250000000000000, 37.32233047033631124, 17.67766952966369232 ) ) ;
#4174 = CARTESIAN_POINT ( 'NONE',  ( -80.00000000000002842, 59.24264068711927678, 11.22792543327563131 ) ) ;
#4175 = CYLINDRICAL_SURFACE ( 'NONE', #9352, 2.500000000000000000 ) ;
#4176 = VECTOR ( 'NONE', #4380, 1000.000000000000000 ) ;
#4177 = ADVANCED_FACE ( 'NONE', ( #8882, #11620 ), #3423, .T. ) ;
#4178 = CARTESIAN_POINT ( 'NONE',  ( -78.00000000000002842, 50.75735931288069480, 14.22792543327563131 ) ) ;
#4179 = CARTESIAN_POINT ( 'NONE',  ( -42.70869921250305623, 54.65600185176862880, -6.994195710570620506 ) ) ;
#4180 = ORIENTED_EDGE ( 'NONE', *, *, #8437, .T. ) ;
#4181 = CARTESIAN_POINT ( 'NONE',  ( -54.63607242817042930, 69.12530316040908929, 15.58420556269393309 ) ) ;
#4182 = CARTESIAN_POINT ( 'NONE',  ( 12.14423903554155793, 49.50741477678717928, 20.43476828740966766 ) ) ;
#4183 = DIRECTION ( 'NONE',  ( 0.000000000000000000, 0.000000000000000000, 1.000000000000000000 ) ) ;
#4184 = CARTESIAN_POINT ( 'NONE',  ( -78.31250000204839523, 29.18810118750000981, 10.69163855873950020 ) ) ;
#4185 = CARTESIAN_POINT ( 'NONE',  ( -1.625240267017640655E-20, 65.42943686846950868, 22.72062601704910634 ) ) ;
#4186 = CARTESIAN_POINT ( 'NONE',  ( -73.71875000204839523, 29.18810118750000271, 4.741568889096522788E-15 ) ) ;
#4187 = EDGE_CURVE ( 'NONE', #4200, #896, #2706, .T. ) ;
#4188 = ADVANCED_FACE ( 'NONE', ( #5584 ), #5349, .F. ) ;
#4189 = ORIENTED_EDGE ( 'NONE', *, *, #8952, .F. ) ;
#4190 = CARTESIAN_POINT ( 'NONE',  ( -73.25000000409677625, 30.00000000000000355, 4.592425496802573578E-15 ) ) ;
#4191 = DIRECTION ( 'NONE',  ( 1.000000000000000000, 6.033820786006286457E-17, -0.000000000000000000 ) ) ;
#4192 = CARTESIAN_POINT ( 'NONE',  ( -75.59374999999990052, 44.64466094068421143, -25.00000000001146105 ) ) ;
#4193 = EDGE_CURVE ( 'NONE', #8389, #2858, #5540, .T. ) ;
#4194 = CARTESIAN_POINT ( 'NONE',  ( -20.50647613538409075, 59.12524989819403487, 20.69783765389080799 ) ) ;
#4195 = CARTESIAN_POINT ( 'NONE',  ( -75.50000000204840944, 29.18810118750000981, 10.69163855873950020 ) ) ;
#4196 = VECTOR ( 'NONE', #3629, 1000.000000000000000 ) ;
#4197 = B_SPLINE_CURVE_WITH_KNOTS ( 'NONE', 3,
 ( #11753, #9125, #8061, #11814, #11636, #10014, #3619, #11703 ),
 .UNSPECIFIED., .F., .F.,
 ( 4, 2, 2, 4 ),
 ( 0.002921158011986720298, 0.003648658599403072685, 0.004376159186819424639, 0.005831160361652126811 ),
 .UNSPECIFIED. ) ;
#4198 = DIRECTION ( 'NONE',  ( -0.000000000000000000, -1.000000000000000000, -0.000000000000000000 ) ) ;
#4199 = CARTESIAN_POINT ( 'NONE',  ( 47.00000000000000000, 47.00000000000000711, 0.000000000000000000 ) ) ;
#4200 = VERTEX_POINT ( 'NONE', #9111 ) ;
#4201 = DIRECTION ( 'NONE',  ( 0.000000000000000000, 1.000000000000000000, 0.000000000000000000 ) ) ;
#4202 = CARTESIAN_POINT ( 'NONE',  ( -76.62500000000000000, 80.00000000000000000, -1.530808498934191324E-15 ) ) ;
#4203 = LINE ( 'NONE', #7862, #10893 ) ;
#4204 = CIRCLE ( 'NONE', #10883, 1.500000000000001332 ) ;
#4205 = DIRECTION ( 'NONE',  ( 0.000000000000000000, 0.000000000000000000, -1.000000000000000000 ) ) ;
#4206 = ORIENTED_EDGE ( 'NONE', *, *, #7278, .F. ) ;
#4207 = CARTESIAN_POINT ( 'NONE',  ( -55.41760771481728653, 58.30620755303042557, 6.186168293415320818 ) ) ;
#4208 = CARTESIAN_POINT ( 'NONE',  ( -78.40625000409677625, 80.00000000000001421, 10.35533905932737397 ) ) ;
#4209 = CARTESIAN_POINT ( 'NONE',  ( -2.500000000000003553, 4.330127018922192761, -6.099999999999999645 ) ) ;
#4210 = AXIS2_PLACEMENT_3D ( 'NONE', #5164, #6911, #8699 ) ;
#4211 = EDGE_LOOP ( 'NONE', ( #8120, #11383, #3138, #10584 ) ) ;
#4212 = CARTESIAN_POINT ( 'NONE',  ( 19.90507239772531634, 75.49690331019444045, 7.999200882884572650 ) ) ;
#4213 = CARTESIAN_POINT ( 'NONE',  ( -78.96875000204839523, 73.25176868561975141, 18.25176868561974075 ) ) ;
#4214 = ORIENTED_EDGE ( 'NONE', *, *, #9599, .T. ) ;
#4215 = CARTESIAN_POINT ( 'NONE',  ( -77.75000000204839523, 65.69163855873948421, -25.81189881250000440 ) ) ;
#4216 = CYLINDRICAL_SURFACE ( 'NONE', #11471, 2.500000000000000000 ) ;
#4217 = CIRCLE ( 'NONE', #6341, 1.500000000000001332 ) ;
#4218 = CARTESIAN_POINT ( 'NONE',  ( -75.12500000409677625, 55.00000000000000000, 24.99999999999999645 ) ) ;
#4219 = CARTESIAN_POINT ( 'NONE',  ( -4.047728495240956903, 54.99641480296497775, 0.008019458024605742932 ) ) ;
#4220 = DIRECTION ( 'NONE',  ( 0.000000000000000000, 0.000000000000000000, 1.000000000000000000 ) ) ;
#4221 = CARTESIAN_POINT ( 'NONE',  ( -74.99999999999998579, 39.36515909056227258, -20.53791299142420712 ) ) ;
#4222 = VECTOR ( 'NONE', #1954, 1000.000000000000000 ) ;
#4223 = VERTEX_POINT ( 'NONE', #11852 ) ;
#4224 = CARTESIAN_POINT ( 'NONE',  ( -2.712167343862823543, -4.207632145829752979, -9.186072312972883233E-16 ) ) ;
#4225 = EDGE_CURVE ( 'NONE', #7521, #2004, #9169, .T. ) ;
#4226 = CIRCLE ( 'NONE', #7681, 1.500000000000001332 ) ;
#4227 = B_SPLINE_CURVE_WITH_KNOTS ( 'NONE', 3,
 ( #10127, #8170, #2776, #10010, #1087, #10912, #5472, #1928, #4575, #11018, #5601, #8284, #8115, #124, #3556, #1805, #1754, #7227, #10855, #6565, #9120, #2661, #904, #8230, #9239, #3790, #1026, #7458, #5532, #9181, #11084, #10194, #10066, #4689, #4515, #2896, #845, #2724, #5, #11811, #3615, #7283, #5656, #6435, #3676, #9292, #1866, #4633, #62, #3727, #7391, #8339, #2168, #2046, #3075, #8404, #8525, #5722, #7632, #2956, #3133, #187, #9602, #3854, #6621, #7748, #11140, #309, #11202, #3012, #9418, #8648 ),
 .UNSPECIFIED., .F., .F.,
 ( 4, 2, 2, 2, 2, 2, 2, 2, 2, 2, 2, 2, 2, 2, 2, 2, 2, 2, 2, 2, 2, 2, 2, 2, 2, 2, 2, 2, 2, 2, 2, 2, 2, 2, 2, 4 ),
 ( 0.06444559019126132327, 0.06662592794032556887, 0.06771609681485769860, 0.06880626568938981447, 0.07098660343845407394, 0.07316694118751831954, 0.07534727893658257902, 0.07752761668564682462, 0.08188829218377530195, 0.08406862993283956142, 0.08624896768190382090, 0.08842930543096806650, 0.08951947430550019624, 0.09060964318003232598, 0.09497031867816085882, 0.09606048755269300243, 0.09715065642722511829, 0.09933099417628937777, 0.1004211630508214936, 0.1015113319253536234, 0.1036916696744178829, 0.1047818385489500126, 0.1058720074234821285, 0.1080523451725464018, 0.1102326829216106613, 0.1113228517961427910, 0.1124130206706749346, 0.1167736961688034397, 0.1189540339178676853, 0.1211343716669319170, 0.1254950471650604360, 0.1276753849141247232, 0.1298557226631889550, 0.1309458915377210986, 0.1320360604122532422, 0.1342163981613174739 ),
 .UNSPECIFIED. ) ;
#4228 = CARTESIAN_POINT ( 'NONE',  ( -50.85567158358731632, 75.98119253013058483, -2.745941642920928683 ) ) ;
#4229 = ORIENTED_EDGE ( 'NONE', *, *, #11821, .F. ) ;
#4230 = CARTESIAN_POINT ( 'NONE',  ( -61.21370359292568253, 51.91450527571464590, 20.80059449010516204 ) ) ;
#4231 = CARTESIAN_POINT ( 'NONE',  ( -33.63031969913447483, 40.99414563559565039, -0.6879892896588567508 ) ) ;
#4232 = CARTESIAN_POINT ( 'NONE',  ( -75.21875000204839523, 36.74823131438024859, -18.25176868561973720 ) ) ;
#4233 = AXIS2_PLACEMENT_3D ( 'NONE', #10424, #2226, #11436 ) ;
#4234 = CIRCLE ( 'NONE', #9959, 1.500000000000001332 ) ;
#4235 = ORIENTED_EDGE ( 'NONE', *, *, #6504, .T. ) ;
#4236 = CARTESIAN_POINT ( 'NONE',  ( -77.18750000204838102, 44.30836144126053000, 25.81189881250000795 ) ) ;
#4237 = CARTESIAN_POINT ( 'NONE',  ( 14.14423903981857755, 49.50929293985068114, 20.43023407247793699 ) ) ;
#4238 = VECTOR ( 'NONE', #5688, 1000.000000000000114 ) ;
#4239 = LINE ( 'NONE', #3334, #5310 ) ;
#4240 = VECTOR ( 'NONE', #2345, 1000.000000000000000 ) ;
#4241 = CARTESIAN_POINT ( 'NONE',  ( -23.16649539194673935, 56.37547255868592799, 6.900582075605663057 ) ) ;
#4242 = EDGE_LOOP ( 'NONE', ( #9934, #11565, #7251, #8253 ) ) ;
#4243 = CARTESIAN_POINT ( 'NONE',  ( -44.39182476880109363, 68.38060868816502591, -16.29271878486493463 ) ) ;
#4244 = CARTESIAN_POINT ( 'NONE',  ( 12.85570563148687739, 52.25434904275299175, 21.01882863504484789 ) ) ;
#4245 = DIRECTION ( 'NONE',  ( -1.000000000000000000, -6.033820786006286457E-17, -0.000000000000000000 ) ) ;
#4246 = CARTESIAN_POINT ( 'NONE',  ( -77.28125000204839523, 73.25176868561975141, 18.25176868561974075 ) ) ;
#4247 =( BOUNDED_CURVE ( )  B_SPLINE_CURVE ( 2, ( #7586, #11214, #3025, #4099, #3199, #10495, #6693, #2119, #5796 ),
 .UNSPECIFIED., .F., .T. ) 
 B_SPLINE_CURVE_WITH_KNOTS ( ( 3, 2, 2, 2, 3 ),
 ( 0.000000000000000000, 0.01979916996583446290, 0.03959833993166892580, 0.05939750989750339216, 0.07919667986333785159 ),
 .UNSPECIFIED. ) 
 CURVE ( )  GEOMETRIC_REPRESENTATION_ITEM ( )  RATIONAL_B_SPLINE_CURVE ( ( 1.000000000000000000, 0.9238795325112868495, 1.000000000000000000, 0.9238795325112868495, 1.000000000000000000, 0.9238795325112868495, 1.000000000000000000, 0.9238795325112868495, 1.000000000000000000 ) ) 
 REPRESENTATION_ITEM ( '' )  );
#4248 = CARTESIAN_POINT ( 'NONE',  ( -78.00000000000001421, 54.99999999999999289, -16.97055937655931501 ) ) ;
#4249 = CARTESIAN_POINT ( 'NONE',  ( -72.59375000204838102, 55.00000000000000000, 25.81189881249999729 ) ) ;
#4250 = ORIENTED_EDGE ( 'NONE', *, *, #5500, .T. ) ;
#4251 = CARTESIAN_POINT ( 'NONE',  ( -72.87500000409677625, 55.00000000000000000, -24.99999999999999645 ) ) ;
#4252 = LINE ( 'NONE', #9926, #1705 ) ;
#4253 = CARTESIAN_POINT ( 'NONE',  ( -71.46875000409677625, 44.64466094067286406, -25.00000000000024869 ) ) ;
#4254 = CARTESIAN_POINT ( 'NONE',  ( -29.54809237377008202, 34.60091625530366599, 5.109976345715927515 ) ) ;
#4255 = EDGE_LOOP ( 'NONE', ( #3628, #10111 ) ) ;
#4256 = CARTESIAN_POINT ( 'NONE',  ( -77.09375000204839523, 36.74823131438026280, 18.25176868561974786 ) ) ;
#4257 = LINE ( 'NONE', #4080, #3576 ) ;
#4258 = EDGE_CURVE ( 'NONE', #8985, #10937, #3478, .T. ) ;
#4259 = DIRECTION ( 'NONE',  ( 0.000000000000000000, 0.000000000000000000, 1.000000000000000000 ) ) ;
#4260 = CARTESIAN_POINT ( 'NONE',  ( -21.32947787934852357, 63.04568470447853912, 19.42265540296757464 ) ) ;
#4261 = LINE ( 'NONE', #7799, #4240 ) ;
#4262 = CARTESIAN_POINT ( 'NONE',  ( -77.56250000204838102, 80.81189881250001861, 10.69163855873948599 ) ) ;
#4263 = CARTESIAN_POINT ( 'NONE',  ( 0.000000000000000000, -30.00000000000000000, 0.000000000000000000 ) ) ;
#4264 = EDGE_LOOP ( 'NONE', ( #1722, #9044 ) ) ;
#4265 = DIRECTION ( 'NONE',  ( -0.000000000000000000, -1.000000000000000000, -0.000000000000000000 ) ) ;
#4266 = PRODUCT_DEFINITION_CONTEXT ( 'detailed design', #10282, 'design' ) ;
#4267 = ORIENTED_EDGE ( 'NONE', *, *, #1808, .T. ) ;
#4268 = EDGE_CURVE ( 'NONE', #5840, #1730, #5775, .T. ) ;
#4269 = CARTESIAN_POINT ( 'NONE',  ( -29.45858744683659936, 48.07282909709525853, 1.028500488243905719 ) ) ;
#4270 = CARTESIAN_POINT ( 'NONE',  ( -77.65624999999998579, 44.64466094066740709, 24.99999999999465672 ) ) ;
#4271 = FACE_OUTER_BOUND ( 'NONE', #8596, .T. ) ;
#4272 = DIRECTION ( 'NONE',  ( 1.000000000000000000, 0.000000000000000000, 0.000000000000000000 ) ) ;
#4273 = CARTESIAN_POINT ( 'NONE',  ( 17.18324390207781960, 73.31587886235929830, -12.20234056926149080 ) ) ;
#4274 = DIRECTION ( 'NONE',  ( 0.000000000000000000, 1.000000000000000000, 0.000000000000000000 ) ) ;
#4275 = ORIENTED_EDGE ( 'NONE', *, *, #8549, .T. ) ;
#4276 = CARTESIAN_POINT ( 'NONE',  ( -75.78125000204839523, 73.25176868561975141, 18.25176868561974075 ) ) ;
#4277 = DIRECTION ( 'NONE',  ( 0.000000000000000000, 0.000000000000000000, -1.000000000000000000 ) ) ;
#4278 = DIRECTION ( 'NONE',  ( -1.000000000000000000, -0.000000000000000000, -0.000000000000000000 ) ) ;
#4279 = CARTESIAN_POINT ( 'NONE',  ( 19.75947799528538340, 54.99150360729431952, -0.02481536840781081721 ) ) ;
#4280 = PRESENTATION_STYLE_ASSIGNMENT (( #9783 ) ) ;
#4281 = DIRECTION ( 'NONE',  ( 0.000000000000000000, 0.000000000000000000, -1.000000000000000000 ) ) ;
#4282 = VERTEX_POINT ( 'NONE', #7564 ) ;
#4283 = CARTESIAN_POINT ( 'NONE',  ( -2.500000000000005773, -4.330127018922191873, 0.000000000000000000 ) ) ;
#4284 = EDGE_CURVE ( 'NONE', #2595, #10896, #919, .T. ) ;
#4285 = CARTESIAN_POINT ( 'NONE',  ( -9.662811212962280294, 69.86524355530642083, -14.86597185903763219 ) ) ;
#4286 = ORIENTED_EDGE ( 'NONE', *, *, #9599, .F. ) ;
#4287 = CARTESIAN_POINT ( 'NONE',  ( -47.14426297200904514, 71.80510559133185211, -12.92232144701529428 ) ) ;
#4288 = CARTESIAN_POINT ( 'NONE',  ( -36.46040627036565951, 42.74970947531311793, -7.056004382930415098 ) ) ;
#4289 = CARTESIAN_POINT ( 'NONE',  ( -78.59375000204839523, 36.74823131438026280, 18.25176868561974786 ) ) ;
#4290 = ORIENTED_EDGE ( 'NONE', *, *, #5660, .T. ) ;
#4291 = CARTESIAN_POINT ( 'NONE',  ( -73.81250000000000000, 72.67766952966368876, -17.67766952966368876 ) ) ;
#4292 = CARTESIAN_POINT ( 'NONE',  ( 6.329456780446692576, 33.97189653527247089, -0.0004287163746460355418 ) ) ;
#4293 = EDGE_LOOP ( 'NONE', ( #7841, #9185, #2241, #2181 ) ) ;
#4294 = DIRECTION ( 'NONE',  ( 0.000000000000000000, -0.000000000000000000, 1.000000000000000000 ) ) ;
#4295 = CARTESIAN_POINT ( 'NONE',  ( 19.99999999999996803, -57.00000000000000000, 5.000000000000000000 ) ) ;
#4296 = CARTESIAN_POINT ( 'NONE',  ( -30.16689009792652243, 49.15416857633141490, 3.904260228111898989 ) ) ;
#4297 = ORIENTED_EDGE ( 'NONE', *, *, #6682, .F. ) ;
#4298 = CARTESIAN_POINT ( 'NONE',  ( 21.18908267236805898, 73.37124140341018119, 10.58130724700091463 ) ) ;
#4299 = EDGE_CURVE ( 'NONE', #7344, #9962, #6737, .T. ) ;
#4300 = CARTESIAN_POINT ( 'NONE',  ( 9.810937555461070048, 42.10554236623130464, 16.77741859935663626 ) ) ;
#4301 = LINE ( 'NONE', #4427, #8118 ) ;
#4302 = DIRECTION ( 'NONE',  ( -1.000000000000000000, -0.000000000000000000, -0.000000000000000000 ) ) ;
#4303 = CARTESIAN_POINT ( 'NONE',  ( -74.75000000204840944, 65.69163855873948421, -25.81189881250000440 ) ) ;
#4304 = ORIENTED_EDGE ( 'NONE', *, *, #8942, .T. ) ;
#4305 = CARTESIAN_POINT ( 'NONE',  ( -73.81250000409677625, 72.67766952966368876, 17.67766952966368521 ) ) ;
#4306 = DIRECTION ( 'NONE',  ( -1.000000000000000000, 0.000000000000000000, -0.000000000000000000 ) ) ;
#4307 = CARTESIAN_POINT ( 'NONE',  ( -66.79101289578984790, 50.03300633731364400, 0.6594954161248131053 ) ) ;
#4308 = PRESENTATION_LAYER_ASSIGNMENT (  '', '', ( #477 ) ) ;
#4309 = CARTESIAN_POINT ( 'NONE',  ( -2.188986190505546769, 52.25407376895000056, -20.97627476078892528 ) ) ;
#4310 = ORIENTED_EDGE ( 'NONE', *, *, #4547, .F. ) ;
#4311 = CARTESIAN_POINT ( 'NONE',  ( -76.62500000204838102, 44.30836144126049447, -25.81189881249999019 ) ) ;
#4312 = CARTESIAN_POINT ( 'NONE',  ( -52.42856357389445066, 59.99999999999997158, -5.034386850915387018E-15 ) ) ;
#4313 = ADVANCED_FACE ( 'NONE', ( #174 ), #3842, .T. ) ;
#4314 =( BOUNDED_CURVE ( )  B_SPLINE_CURVE ( 2, ( #1450, #4270, #11502, #7807, #7870, #10601, #7983, #1509, #4327 ),
 .UNSPECIFIED., .F., .T. ) 
 B_SPLINE_CURVE_WITH_KNOTS ( ( 3, 2, 2, 2, 3 ),
 ( 0.2376281879409543607, 0.2574394709827818040, 0.2772507540246093027, 0.2970620370664368015, 0.3168733201082642448 ),
 .UNSPECIFIED. ) 
 CURVE ( )  GEOMETRIC_REPRESENTATION_ITEM ( )  RATIONAL_B_SPLINE_CURVE ( ( 0.9999999999999494849, 0.9238795325113373647, 1.000000000000000000, 0.9238795325112868495, 1.000000000000000000, 0.9238795325112868495, 1.000000000000000000, 0.9238795325112868495, 1.000000000000000000 ) ) 
 REPRESENTATION_ITEM ( '' )  );
#4315 = DIRECTION ( 'NONE',  ( 0.000000000000000000, -0.000000000000000000, 1.000000000000000000 ) ) ;
#4316=STYLED_ITEM('',(#11895),#684);
#4317 = CARTESIAN_POINT ( 'NONE',  ( -44.07074648197151845, 61.10275710191199749, -20.11236068975357938 ) ) ;
#4318 = DIRECTION ( 'NONE',  ( -1.000000000000000000, -0.000000000000000000, -0.000000000000000000 ) ) ;
#4319 = CARTESIAN_POINT ( 'NONE',  ( -78.87500000204838102, 65.69163855873949842, 25.81189881250000440 ) ) ;
#4320 = CARTESIAN_POINT ( 'NONE',  ( -80.00000000000000000, 55.00000000000000000, 0.000000000000000000 ) ) ;
#4321 = ORIENTED_EDGE ( 'NONE', *, *, #2774, .T. ) ;
#4322 = CARTESIAN_POINT ( 'NONE',  ( 5.000000000000000000, -2.886751345948136205, -6.099999999999999645 ) ) ;
#4323 = EDGE_LOOP ( 'NONE', ( #5427, #10538, #4909 ) ) ;
#4324 = EDGE_CURVE ( 'NONE', #388, #6710, #2944, .T. ) ;
#4325 = CARTESIAN_POINT ( 'NONE',  ( -36.55667896093988389, 51.48427161832111665, -6.093033236249906004 ) ) ;
#4326 =( REPRESENTATION_RELATIONSHIP ('NONE','NONE', #5489, #2176 ) REPRESENTATION_RELATIONSHIP_WITH_TRANSFORMATION ( #8169 )SHAPE_REPRESENTATION_RELATIONSHIP( ) );
#4327 = CARTESIAN_POINT ( 'NONE',  ( -77.00000000000000000, 55.00000000000000000, -24.99999999999999645 ) ) ;
#4328 = PRODUCT_RELATED_PRODUCT_CATEGORY ( 'part', '', ( #10530 ) ) ;
#4329 = CARTESIAN_POINT ( 'NONE',  ( -77.09375000409677625, 80.00000000000001421, -10.35533905932737753 ) ) ;
#4330 = EDGE_CURVE ( 'NONE', #9331, #6771, #7509, .T. ) ;
#4331 = AXIS2_PLACEMENT_3D ( 'NONE', #1878, #9192, #4645 ) ;
#4332 = EDGE_CURVE ( 'NONE', #9420, #8886, #5709, .T. ) ;
#4333 = ADVANCED_FACE ( 'NONE', ( #8577 ), #1975, .F. ) ;
#4334 = CARTESIAN_POINT ( 'NONE',  ( 19.13801014043440318, 74.86951949782532267, -9.538400742199257820 ) ) ;
#4335 = CARTESIAN_POINT ( 'NONE',  ( -71.59560441993424718, 80.81189881250001861, 6.916273537586018705 ) ) ;
#4336 = ORIENTED_EDGE ( 'NONE', *, *, #8896, .T. ) ;
#4337 = AXIS2_PLACEMENT_3D ( 'NONE', #11160, #65, #8471 ) ;
#4338 = CARTESIAN_POINT ( 'NONE',  ( -74.65625000204839523, 73.25176868561975141, -18.25176868561974430 ) ) ;
#4339 = CARTESIAN_POINT ( 'NONE',  ( -5.000000000000000000, 2.419979747126323577, -0.3118366332702841026 ) ) ;
#4340 = EDGE_CURVE ( 'NONE', #4456, #6484, #7, .T. ) ;
#4341 = ADVANCED_FACE ( 'NONE', ( #4985, #354 ), #8636, .F. ) ;
#4342 = FACE_OUTER_BOUND ( 'NONE', #10677, .T. ) ;
#4343 = CARTESIAN_POINT ( 'NONE',  ( 22.09282151157359309, 54.98265345718393604, -0.01967570506841854680 ) ) ;
#4344 = CARTESIAN_POINT ( 'NONE',  ( 0.000000000000000000, 0.000000000000000000, 0.000000000000000000 ) ) ;
#4345 = CARTESIAN_POINT ( 'NONE',  ( -75.00000000000000000, 32.46325592683887606, 11.40855839108016667 ) ) ;
#4346 = ADVANCED_FACE ( 'NONE', ( #10363 ), #7621, .F. ) ;
#4347 = CIRCLE ( 'NONE', #5119, 5.249999999999998224 ) ;
#4348 = ORIENTED_EDGE ( 'NONE', *, *, #11280, .F. ) ;
#4349 = CARTESIAN_POINT ( 'NONE',  ( 0.000000000000000000, -24.99999999999999645, 0.000000000000000000 ) ) ;
#4350 = CARTESIAN_POINT ( 'NONE',  ( -55.45210586135002728, 71.88485191958531573, 12.52183031059725771 ) ) ;
#4351 = ORIENTED_EDGE ( 'NONE', *, *, #6323, .F. ) ;
#4352 = CARTESIAN_POINT ( 'NONE',  ( -28.82693382303331475, 37.45538988585808937, 11.71519277693090366 ) ) ;
#4353 = CARTESIAN_POINT ( 'NONE',  ( -45.29698632460738139, 60.99542764961179842, -12.67644002407605086 ) ) ;
#4354 = CARTESIAN_POINT ( 'NONE',  ( -78.31250000204838102, 29.18810118750000626, -10.69163855873949309 ) ) ;
#4355 = AXIS2_PLACEMENT_3D ( 'NONE', #1185, #3828, #1058 ) ;
#4356 = CIRCLE ( 'NONE', #1281, 4.000000000000003553 ) ;
#4357 = ORIENTED_EDGE ( 'NONE', *, *, #3062, .T. ) ;
#4358 = CARTESIAN_POINT ( 'NONE',  ( -79.15625000204838102, 80.81189881250000440, -1.580522963032174394E-15 ) ) ;
#4359 = CARTESIAN_POINT ( 'NONE',  ( 4.881307793505825110, 34.60946683332392126, -5.106800360247272685 ) ) ;
#4360 = DIRECTION ( 'NONE',  ( -1.000000000000000000, -0.000000000000000000, -0.000000000000000000 ) ) ;
#4361 = CARTESIAN_POINT ( 'NONE',  ( 8.654567787479487961, 50.16095913586803334, 1.299965765103639148 ) ) ;
#4362 = CARTESIAN_POINT ( 'NONE',  ( 11.90727647329997829, 54.99834172827340240, 0.01637095017119612195 ) ) ;
#4363 = MECHANICAL_DESIGN_GEOMETRIC_PRESENTATION_REPRESENTATION (  '', ( #6669 ), #2050 ) ;
#4364 = ORIENTED_EDGE ( 'NONE', *, *, #3449, .T. ) ;
#4365 = CARTESIAN_POINT ( 'NONE',  ( -67.52720549794999272, 34.02364409886038743, 2.748840581154547102 ) ) ;
#4366 = CARTESIAN_POINT ( 'NONE',  ( 39.99999999999999289, 55.00000000000000000, 24.99999999999999645 ) ) ;
#4367 = DIRECTION ( 'NONE',  ( -0.000000000000000000, -0.000000000000000000, 1.000000000000000000 ) ) ;
#4368 = DIRECTION ( 'NONE',  ( 1.000000000000000000, 6.033820786006286457E-17, -0.000000000000000000 ) ) ;
#4369 = CARTESIAN_POINT ( 'NONE',  ( -72.31250000204839523, 29.18810118750000981, 10.69163855873950020 ) ) ;
#4370 = ORIENTED_EDGE ( 'NONE', *, *, #1191, .F. ) ;
#4371 = CARTESIAN_POINT ( 'NONE',  ( -75.21875000409677625, 65.35533905932737753, 24.99999999999999645 ) ) ;
#4372 = DIRECTION ( 'NONE',  ( 0.000000000000000000, 0.000000000000000000, 1.000000000000000000 ) ) ;
#4373 = FACE_BOUND ( 'NONE', #4255, .T. ) ;
#4374 = VECTOR ( 'NONE', #7623, 1000.000000000000000 ) ;
#4375 = CARTESIAN_POINT ( 'NONE',  ( -55.50627899214600092, 66.73177265193905328, 17.54361557889675893 ) ) ;
#4376 = ORIENTED_EDGE ( 'NONE', *, *, #6831, .F. ) ;
#4377 = CARTESIAN_POINT ( 'NONE',  ( -77.46875000204839523, 73.25176868561975141, 18.25176868561974075 ) ) ;
#4378 = CARTESIAN_POINT ( 'NONE',  ( -3.000000000000000000, 0.000000000000000000, -0.02539999999999996774 ) ) ;
#4379 = EDGE_CURVE ( 'NONE', #5071, #131, #9971, .T. ) ;
#4380 = DIRECTION ( 'NONE',  ( 1.000000000000000000, 6.033820786006286457E-17, -0.000000000000000000 ) ) ;
#4381 = DIRECTION ( 'NONE',  ( 0.000000000000000000, 1.000000000000000000, 0.000000000000000000 ) ) ;
#4382 = CARTESIAN_POINT ( 'NONE',  ( -74.93750000204839523, 65.69163855873948421, -25.81189881250000440 ) ) ;
#4383 = CARTESIAN_POINT ( 'NONE',  ( -78.00000000000001421, 67.72792206135787296, -12.72791868944004534 ) ) ;
#4384 = ORIENTED_EDGE ( 'NONE', *, *, #4529, .F. ) ;
#4385 = CARTESIAN_POINT ( 'NONE',  ( 14.99999999999999645, 55.00000000000000000, 0.000000000000000000 ) ) ;
#4386 = VERTEX_POINT ( 'NONE', #10534 ) ;
#4387 = CARTESIAN_POINT ( 'NONE',  ( 24.78347237616896237, 79.56634503030461758, 4.655107467241123231 ) ) ;
#4388 = AXIS2_PLACEMENT_3D ( 'NONE', #8676, #7897, #7002 ) ;
#4389 = CARTESIAN_POINT ( 'NONE',  ( 9.793834090903223100, 42.78911815673161811, 7.039953125326757544 ) ) ;
#4390 = CARTESIAN_POINT ( 'NONE',  ( -71.03052368859394505, 76.88501343918500197, 12.63531067400213104 ) ) ;
#4391 = CARTESIAN_POINT ( 'NONE',  ( 36.99999999999999289, 55.00000000000000000, 5.249999999999998224 ) ) ;
#4392 = DIRECTION ( 'NONE',  ( 0.000000000000000000, 0.000000000000000000, 1.000000000000000000 ) ) ;
#4393 = CONICAL_SURFACE ( 'NONE', #3623, 2.500000000000000000, 0.9599310885968755924 ) ;
#4394 = CARTESIAN_POINT ( 'NONE',  ( 36.99999999999999289, 55.00000000000000000, 0.000000000000000000 ) ) ;
#4395 = AXIS2_PLACEMENT_3D ( 'NONE', #5551, #207, #1103 ) ;
#4396 = ORIENTED_EDGE ( 'NONE', *, *, #10917, .F. ) ;
#4397 = SURFACE_STYLE_USAGE ( .BOTH. , #8949 ) ;
#4398 = CARTESIAN_POINT ( 'NONE',  ( -74.28125000204839523, 73.25176868561975141, 18.25176868561974075 ) ) ;
#4399 = DIRECTION ( 'NONE',  ( 0.000000000000000000, 1.000000000000000000, 0.000000000000000000 ) ) ;
#4400 = UNCERTAINTY_MEASURE_WITH_UNIT (LENGTH_MEASURE( 1.000000000000000082E-05 ), #4417, 'distance_accuracy_value', 'NONE');
#4401 = DIRECTION ( 'NONE',  ( -1.000000000000000000, -6.033820786006286457E-17, -0.000000000000000000 ) ) ;
#4402 = DIRECTION ( 'NONE',  ( 1.000000000000000000, 0.000000000000000000, 0.000000000000000000 ) ) ;
#4403 = VECTOR ( 'NONE', #3637, 1000.000000000000000 ) ;
#4404 = DIRECTION ( 'NONE',  ( 1.000000000000000000, 0.000000000000000000, 0.000000000000000000 ) ) ;
#4405 = CIRCLE ( 'NONE', #3826, 21.50000000000000000 ) ;
#4406 = CARTESIAN_POINT ( 'NONE',  ( -74.99999999999994316, 33.80523199205565277, 13.63254922431209870 ) ) ;
#4407 = ORIENTED_EDGE ( 'NONE', *, *, #7782, .F. ) ;
#4408 = CARTESIAN_POINT ( 'NONE',  ( -18.18548385789268451, 57.21583455123535344, 4.494158473437730450 ) ) ;
#4409 = EDGE_CURVE ( 'NONE', #1675, #3592, #4048, .T. ) ;
#4410 = DIRECTION ( 'NONE',  ( 0.000000000000000000, -0.000000000000000000, -1.000000000000000000 ) ) ;
#4411 = ORIENTED_EDGE ( 'NONE', *, *, #5652, .F. ) ;
#4412 = CARTESIAN_POINT ( 'NONE',  ( -34.05849041764468410, 34.82468742385552218, -6.128056420806536231 ) ) ;
#4413 = CARTESIAN_POINT ( 'NONE',  ( -76.71875000204839523, 36.74823131438024859, -18.25176868561973720 ) ) ;
#4414 = ORIENTED_EDGE ( 'NONE', *, *, #8576, .T. ) ;
#4415 = CARTESIAN_POINT ( 'NONE',  ( -74.00000000204839523, 29.18810118750000981, 10.69163855873950020 ) ) ;
#4416 = DIRECTION ( 'NONE',  ( -0.000000000000000000, -1.000000000000000000, -0.000000000000000000 ) ) ;
#4417 =( LENGTH_UNIT ( ) NAMED_UNIT ( * ) SI_UNIT ( .MILLI., .METRE. ) );
#4418 = ADVANCED_FACE ( 'NONE', ( #10707 ), #5012, .F. ) ;
#4419 = ADVANCED_FACE ( 'NONE', ( #9588 ), #2273, .F. ) ;
#4420 = CARTESIAN_POINT ( 'NONE',  ( -2.500000000000000000, 3.061616997868383141E-16, -6.099999999999999645 ) ) ;
#4421 = CARTESIAN_POINT ( 'NONE',  ( 14.48524493375191291, 53.39293360022251278, 4.746189266409619023 ) ) ;
#4422 = CARTESIAN_POINT ( 'NONE',  ( -57.29127706180261725, 59.71020960438666236, 5.197211960637448058 ) ) ;
#4423 = ORIENTED_EDGE ( 'NONE', *, *, #7927, .F. ) ;
#4424 = CARTESIAN_POINT ( 'NONE',  ( 18.85563813666183819, 67.92324243781868631, 16.80650911442449313 ) ) ;
#4425 = VECTOR ( 'NONE', #7363, 1000.000000000000000 ) ;
#4426 = CARTESIAN_POINT ( 'NONE',  ( -9.662811212962280294, 69.86524355530642083, -14.86597185903763219 ) ) ;
#4427 = CARTESIAN_POINT ( 'NONE',  ( -75.00000000000000000, 55.00000000000000000, 25.00000000000000355 ) ) ;
#4428 = DIRECTION ( 'NONE',  ( -1.000000000000000000, 0.000000000000000000, 0.000000000000000000 ) ) ;
#4429 = CARTESIAN_POINT ( 'NONE',  ( -83.00000000000000000, 55.00000000000000000, 0.000000000000000000 ) ) ;
#4430 = EDGE_LOOP ( 'NONE', ( #1513, #908 ) ) ;
#4431 = DIRECTION ( 'NONE',  ( 0.9999998346844722885, -0.0005712585774195265247, 6.553370117834432030E-05 ) ) ;
#4432 = DIRECTION ( 'NONE',  ( -1.000000000000000000, -0.000000000000000000, -0.000000000000000000 ) ) ;
#4433 = PLANE ( 'NONE',  #4057 ) ;
#4434 = CARTESIAN_POINT ( 'NONE',  ( -41.78535879711923684, 60.10680040617825881, -20.39053309953287751 ) ) ;
#4435 = VECTOR ( 'NONE', #5668, 1000.000000000000000 ) ;
#4436 = ORIENTED_EDGE ( 'NONE', *, *, #8942, .F. ) ;
#4437 = AXIS2_PLACEMENT_3D ( 'NONE', #2351, #11558, #7155 ) ;
#4438 = FACE_OUTER_BOUND ( 'NONE', #9300, .T. ) ;
#4439 = CARTESIAN_POINT ( 'NONE',  ( -60.20667922569305830, 56.29624695176077864, 4.839977866460043465 ) ) ;
#4440 = ORIENTED_EDGE ( 'NONE', *, *, #10537, .T. ) ;
#4441 = EDGE_CURVE ( 'NONE', #4164, #11218, #6547, .T. ) ;
#4442 = DIRECTION ( 'NONE',  ( 2.126576849575776229E-17, 0.9848077530122080203, -0.1736481776669307198 ) ) ;
#4443 = DIRECTION ( 'NONE',  ( 0.000000000000000000, 1.000000000000000000, 0.000000000000000000 ) ) ;
#4444 = CARTESIAN_POINT ( 'NONE',  ( -77.00000000204838102, 29.18810118750000981, 10.69163855873950020 ) ) ;
#4445 = CONICAL_SURFACE ( 'NONE', #9212, 4.000000000000003553, 0.05235987755983000091 ) ;
#4446 = CARTESIAN_POINT ( 'NONE',  ( -74.75000000204839523, 80.81189881250001861, -10.69163855873949132 ) ) ;
#4447 = ORIENTED_EDGE ( 'NONE', *, *, #3131, .T. ) ;
#4448 = LINE ( 'NONE', #9765, #3087 ) ;
#4449 = ORIENTED_EDGE ( 'NONE', *, *, #11785, .F. ) ;
#4450 = CARTESIAN_POINT ( 'NONE',  ( 0.4815530525298790665, 52.78317629943902034, -4.493698677454305290 ) ) ;
#4451 = CARTESIAN_POINT ( 'NONE',  ( -22.12707294284022197, 53.16908462427974769, 14.02455705437751909 ) ) ;
#4452 = CARTESIAN_POINT ( 'NONE',  ( -79.06250000204840944, 80.81189881250000440, -10.69163855873948954 ) ) ;
#4453 = DIRECTION ( 'NONE',  ( -0.8191520442889885789, 1.003171929053520802E-16, 0.5735764363510507113 ) ) ;
#4454 = CARTESIAN_POINT ( 'NONE',  ( -83.00000000000000000, 55.00000000000000000, 0.000000000000000000 ) ) ;
#4455 = DIRECTION ( 'NONE',  ( 1.000000000000000000, 0.000000000000000000, 0.000000000000000000 ) ) ;
#4456 = VERTEX_POINT ( 'NONE', #8923 ) ;
#4457 = ADVANCED_FACE ( 'NONE', ( #5949 ), #9642, .T. ) ;
#4458 = CARTESIAN_POINT ( 'NONE',  ( -77.93750000204838102, 44.30836144126050158, -25.81189881249999374 ) ) ;
#4459 = CARTESIAN_POINT ( 'NONE',  ( -80.00000000000001421, 67.72792206135787296, 2.742644059037073312 ) ) ;
#4460 = EDGE_CURVE ( 'NONE', #10478, #9989, #7990, .T. ) ;
#4461 = CARTESIAN_POINT ( 'NONE',  ( -80.00000000000000000, 55.00000000000000000, 20.00000000000000355 ) ) ;
#4462 = CARTESIAN_POINT ( 'NONE',  ( -22.24059675286479276, 55.01153819220757413, -0.02355272863444527257 ) ) ;
#4463 = CARTESIAN_POINT ( 'NONE',  ( 2.500000000000005773, 4.330127018922190985, -6.099999999999999645 ) ) ;
#4464 = ORIENTED_EDGE ( 'NONE', *, *, #3862, .T. ) ;
#4465 = CARTESIAN_POINT ( 'NONE',  ( -20.00000000000003197, -63.00000000000000000, 5.000000000000000000 ) ) ;
#4466 = ADVANCED_FACE ( 'NONE', ( #9871 ), #6242, .T. ) ;
#4467 = CARTESIAN_POINT ( 'NONE',  ( -59.82750509709391196, 59.10995506582904824, 20.69284243654335498 ) ) ;
#4468 = ORIENTED_EDGE ( 'NONE', *, *, #2675, .F. ) ;
#4469 = CARTESIAN_POINT ( 'NONE',  ( -56.83961221553562382, 66.73132451083796468, 17.54318035443342438 ) ) ;
#4470 = CARTESIAN_POINT ( 'NONE',  ( -74.84375000204839523, 73.25176868561975141, -18.25176868561974430 ) ) ;
#4471 = ORIENTED_EDGE ( 'NONE', *, *, #10184, .T. ) ;
#4472 = CARTESIAN_POINT ( 'NONE',  ( -72.03125000204838102, 55.00000000000000000, -25.81189881249999729 ) ) ;
#4473 = CARTESIAN_POINT ( 'NONE',  ( -5.929357825456832209, 64.91315550346766372, -18.55154749960842153 ) ) ;
#4474 =( LENGTH_UNIT ( ) NAMED_UNIT ( * ) SI_UNIT ( .MILLI., .METRE. ) );
#4475 = DIRECTION ( 'NONE',  ( -0.000000000000000000, -0.000000000000000000, -1.000000000000000000 ) ) ;
#4476 = CARTESIAN_POINT ( 'NONE',  ( -5.240525354424131699, 54.99835323915754515, 0.01636088839724062979 ) ) ;
#4477 = ORIENTED_EDGE ( 'NONE', *, *, #6659, .F. ) ;
#4478 = CARTESIAN_POINT ( 'NONE',  ( 9.522371807443699154, 38.19365890154983845, 12.92340179382780896 ) ) ;
#4479 = CARTESIAN_POINT ( 'NONE',  ( -6.160267096003628318, 59.12214581854949103, -20.69010011304746044 ) ) ;
#4480 = CARTESIAN_POINT ( 'NONE',  ( 5.000000000000000888, -1.936377641173860686, -5.902630826755077997 ) ) ;
#4481 = CYLINDRICAL_SURFACE ( 'NONE', #2473, 4.999999999999984013 ) ;
#4482 = AXIS2_PLACEMENT_3D ( 'NONE', #2380, #8800, #10632 ) ;
#4483 = CARTESIAN_POINT ( 'NONE',  ( 0.000000000000000000, 0.000000000000000000, -2.267810516609437776 ) ) ;
#4484 = EDGE_LOOP ( 'NONE', ( #5701, #4649, #3390, #7006 ) ) ;
#4485 = CARTESIAN_POINT ( 'NONE',  ( -76.34375000000005684, 65.35533905932732068, 24.99999999999990052 ) ) ;
#4486 = DIRECTION ( 'NONE',  ( 0.000000000000000000, 0.000000000000000000, 1.000000000000000000 ) ) ;
#4487 = CARTESIAN_POINT ( 'NONE',  ( 0.000000000000000000, 5.000000000000000000, 0.000000000000000000 ) ) ;
#4488 = ORIENTED_EDGE ( 'NONE', *, *, #946, .T. ) ;
#4489 = DIRECTION ( 'NONE',  ( 0.000000000000000000, 0.000000000000000000, -1.000000000000000000 ) ) ;
#4490 = EDGE_CURVE ( 'NONE', #7952, #5996, #211, .T. ) ;
#4491 = DIRECTION ( 'NONE',  ( -1.000000000000000000, -0.000000000000000000, -0.000000000000000000 ) ) ;
#4492 = VERTEX_POINT ( 'NONE', #9095 ) ;
#4493 = DIRECTION ( 'NONE',  ( -1.000000000000000000, -0.000000000000000000, -0.000000000000000000 ) ) ;
#4494 = LINE ( 'NONE', #1064, #9373 ) ;
#4495 = PLANE ( 'NONE',  #10458 ) ;
#4496 = CARTESIAN_POINT ( 'NONE',  ( -78.68750000204838102, 44.30836144126053000, 25.81189881250000795 ) ) ;
#4497 = DIRECTION ( 'NONE',  ( -0.000000000000000000, -0.000000000000000000, -1.000000000000000000 ) ) ;
#4498 =( GEOMETRIC_REPRESENTATION_CONTEXT ( 3 ) GLOBAL_UNCERTAINTY_ASSIGNED_CONTEXT ( ( #670 ) ) GLOBAL_UNIT_ASSIGNED_CONTEXT ( ( #7474, #6756, #3985 ) ) REPRESENTATION_CONTEXT ( 'NONE', 'WORKASPACE' ) );
#4499 = ORIENTED_EDGE ( 'NONE', *, *, #10336, .T. ) ;
#4500 = CARTESIAN_POINT ( 'NONE',  ( -75.12500000204838102, 29.18810118750000626, -10.69163855873949309 ) ) ;
#4501 = EDGE_LOOP ( 'NONE', ( #3896, #5187, #1565, #9674, #2696 ) ) ;
#4502 = CARTESIAN_POINT ( 'NONE',  ( 6.634799041927093910, 66.87503529737901431, 22.00033049848320488 ) ) ;
#4503 = CARTESIAN_POINT ( 'NONE',  ( 4.922725082627545490, 41.59604121305380886, -4.066663295143957413 ) ) ;
#4504 = CARTESIAN_POINT ( 'NONE',  ( -75.96875000204839523, 80.81189881250000440, -1.580522963032174394E-15 ) ) ;
#4505 = CARTESIAN_POINT ( 'NONE',  ( -77.00000000409677625, 80.00000000000000000, -1.530808498934191324E-15 ) ) ;
#4506 = DIRECTION ( 'NONE',  ( 1.000000000000000000, -0.000000000000000000, -0.000000000000000000 ) ) ;
#4507 = ORIENTED_EDGE ( 'NONE', *, *, #10614, .F. ) ;
#4508 = FILL_AREA_STYLE_COLOUR ( '', #2971 ) ;
#4509 = CARTESIAN_POINT ( 'NONE',  ( -77.09375000409677625, 80.00000000000001421, -10.35533905932737753 ) ) ;
#4510 = DIRECTION ( 'NONE',  ( 0.000000000000000000, 1.000000000000000000, 0.000000000000000000 ) ) ;
#4511 = ORIENTED_EDGE ( 'NONE', *, *, #9828, .F. ) ;
#4512 = DIRECTION ( 'NONE',  ( -0.000000000000000000, -0.000000000000000000, 1.000000000000000000 ) ) ;
#4513 = CARTESIAN_POINT ( 'NONE',  ( -52.46182469558537775, 54.99624011979340565, -0.004044406450102152988 ) ) ;
#4514 = SHAPE_DEFINITION_REPRESENTATION ( #489, #5489 ) ;
#4515 = CARTESIAN_POINT ( 'NONE',  ( -21.71309743435359962, 76.99877995635615946, -0.7660633642738442495 ) ) ;
#4516 = CIRCLE ( 'NONE', #6064, 1.500000000000001332 ) ;
#4517 = CARTESIAN_POINT ( 'NONE',  ( -11.57142270279487306, 60.00000000000001421, -4.065933922700817035E-15 ) ) ;
#4518 = ORIENTED_EDGE ( 'NONE', *, *, #8804, .T. ) ;
#4519 = CARTESIAN_POINT ( 'NONE',  ( -66.47562283042974229, 38.19906477560226676, 12.92409071120044040 ) ) ;
#4520 = ORIENTED_EDGE ( 'NONE', *, *, #75, .F. ) ;
#4521 = ADVANCED_FACE ( 'NONE', ( #4438 ), #977, .F. ) ;
#4522 = CARTESIAN_POINT ( 'NONE',  ( -11.39182375260447166, 73.60042400440836730, -9.933379572949093017 ) ) ;
#4523 = CARTESIAN_POINT ( 'NONE',  ( -72.40625000204838102, 29.18810118750000271, 4.741568889096522788E-15 ) ) ;
#4524 = CIRCLE ( 'NONE', #1546, 1.500000000000001332 ) ;
#4525 = EDGE_CURVE ( 'NONE', #10937, #5713, #6299, .T. ) ;
#4526 = ORIENTED_EDGE ( 'NONE', *, *, #11204, .F. ) ;
#4527 = CARTESIAN_POINT ( 'NONE',  ( -75.87500000204839523, 65.69163855873949842, 25.81189881250000440 ) ) ;
#4528 = CARTESIAN_POINT ( 'NONE',  ( -30.11869220662914159, 34.20731585996448132, 3.085050890631813036 ) ) ;
#4529 = EDGE_CURVE ( 'NONE', #7593, #9403, #6357, .T. ) ;
#4530 = EDGE_LOOP ( 'NONE', ( #6309, #11675 ) ) ;
#4531 = CARTESIAN_POINT ( 'NONE',  ( 3.000000000000000888, 0.000000000000000000, -25.03750572909317285 ) ) ;
#4532 = CARTESIAN_POINT ( 'NONE',  ( 15.75947798662055988, 54.99526034255116258, -0.01574567900935226750 ) ) ;
#4533 = ORIENTED_EDGE ( 'NONE', *, *, #3418, .F. ) ;
#4534 = CARTESIAN_POINT ( 'NONE',  ( 24.33333333333332149, 76.00000000000000000, 0.000000000000000000 ) ) ;
#4535 = AXIS2_PLACEMENT_3D ( 'NONE', #1075, #2099, #3903 ) ;
#4536 = CARTESIAN_POINT ( 'NONE',  ( -15.14429485721040614, 76.01882847486140804, 2.745652427074330326 ) ) ;
#4537 = DIRECTION ( 'NONE',  ( -1.000000000000000000, -0.000000000000000000, -0.000000000000000000 ) ) ;
#4538 = CARTESIAN_POINT ( 'NONE',  ( 63.00000000000000000, 55.00000000000000000, 2.445500000000003116 ) ) ;
#4539 = AXIS2_PLACEMENT_3D ( 'NONE', #5131, #10501, #11454 ) ;
#4540 = DIRECTION ( 'NONE',  ( 0.000000000000000000, 0.000000000000000000, 1.000000000000000000 ) ) ;
#4541 = DIRECTION ( 'NONE',  ( 0.000000000000000000, 1.000000000000000000, 0.000000000000000000 ) ) ;
#4542 = ORIENTED_EDGE ( 'NONE', *, *, #6385, .F. ) ;
#4543 = DIRECTION ( 'NONE',  ( 6.527513432760042190E-05, -0.0004526335343839516683, -0.9999998954310147514 ) ) ;
#4544 = CARTESIAN_POINT ( 'NONE',  ( -32.24307070243303741, 54.99420864160337885, 0.001526422163665167291 ) ) ;
#4545 = PRODUCT_DEFINITION ( 'UNKNOWN', '', #5096, #8822 ) ;
#4546 = CARTESIAN_POINT ( 'NONE',  ( -50.84658144432280125, 59.74596735251822821, 1.607341111116408428 ) ) ;
#4547 = EDGE_CURVE ( 'NONE', #6864, #8080, #9402, .T. ) ;
#4548 = CIRCLE ( 'NONE', #2814, 2.500000000000000000 ) ;
#4549 = PLANE ( 'NONE',  #597 ) ;
#4550 = CARTESIAN_POINT ( 'NONE',  ( -56.71072052760479920, 58.76569921069902591, 3.305499569647178060 ) ) ;
#4551 = VERTEX_POINT ( 'NONE', #2805 ) ;
#4552 = LINE ( 'NONE', #4728, #11431 ) ;
#4553 = ADVANCED_FACE ( 'NONE', ( #11667 ), #4549, .T. ) ;
#4554 = CARTESIAN_POINT ( 'NONE',  ( 52.99999999999999289, 58.53553390593273065, 3.535533905932731091 ) ) ;
#4555 = EDGE_CURVE ( 'NONE', #7093, #3681, #3276, .T. ) ;
#4556 = LINE ( 'NONE', #9159, #2622 ) ;
#4557 = CARTESIAN_POINT ( 'NONE',  ( -71.75000000204838102, 80.81189881250001861, -10.69163855873949132 ) ) ;
#4558 = CARTESIAN_POINT ( 'NONE',  ( -77.09375000204839523, 36.74823131438026280, 18.25176868561974786 ) ) ;
#4559 = CIRCLE ( 'NONE', #3598, 20.00000000000000355 ) ;
#4560 = ORIENTED_EDGE ( 'NONE', *, *, #6659, .T. ) ;
#4561 = CARTESIAN_POINT ( 'NONE',  ( -74.84375000204839523, 55.00000000000000000, -25.81189881249999729 ) ) ;
#4562 = ORIENTED_EDGE ( 'NONE', *, *, #10075, .T. ) ;
#4563 = CARTESIAN_POINT ( 'NONE',  ( 24.28641463743580786, 79.14216019722405804, 6.705329215194802295 ) ) ;
#4564 = CARTESIAN_POINT ( 'NONE',  ( -5.878133643754496873, 62.20801019244017027, -12.02644650578262997 ) ) ;
#4565 = ADVANCED_FACE ( 'NONE', ( #8201 ), #1898, .T. ) ;
#4566 = ADVANCED_BREP_SHAPE_REPRESENTATION ( '', ( #4740, #4738 ), #844 ) ;
#4567 = CARTESIAN_POINT ( 'NONE',  ( -78.68750000204839523, 65.69163855873949842, 25.81189881250000084 ) ) ;
#4568 = CARTESIAN_POINT ( 'NONE',  ( 0.8192951148925836646, -5.300482436767290473, -5.901655677627834606 ) ) ;
#4569 = CARTESIAN_POINT ( 'NONE',  ( -78.00000000000000000, 55.00000000000000000, 0.000000000000000000 ) ) ;
#4570 = EDGE_LOOP ( 'NONE', ( #11040, #8302, #1484, #8922 ) ) ;
#4571 = CARTESIAN_POINT ( 'NONE',  ( -78.87500000409677625, 55.00000000000000000, -24.99999999999999645 ) ) ;
#4572 = CYLINDRICAL_SURFACE ( 'NONE', #4801, 1.499999999999999556 ) ;
#4573 = CARTESIAN_POINT ( 'NONE',  ( -40.79520177461022001, 54.99765425461028912, 0.005074365896716425024 ) ) ;
#4574 = PRODUCT_CONTEXT ( 'NONE', #10659, 'mechanical' ) ;
#4575 = CARTESIAN_POINT ( 'NONE',  ( -5.679186637561253193, 66.13248820997100097, -18.97822730947832781 ) ) ;
#4576 = DIRECTION ( 'NONE',  ( -1.000000000000000000, -0.000000000000000000, -0.000000000000000000 ) ) ;
#4577 = MECHANICAL_DESIGN_GEOMETRIC_PRESENTATION_REPRESENTATION (  '', ( #3801 ), #8019 ) ;
#4578 = VERTEX_POINT ( 'NONE', #3646 ) ;
#4579 = EDGE_LOOP ( 'NONE', ( #9581, #6344, #2846, #4755 ) ) ;
#4580 = CARTESIAN_POINT ( 'NONE',  ( -17.27494751259140315, 73.62640980466187557, 9.944421848179040069 ) ) ;
#4581 = CARTESIAN_POINT ( 'NONE',  ( -79.25000000204838102, 65.69163855873948421, -25.81189881250000440 ) ) ;
#4582 = VECTOR ( 'NONE', #11162, 1000.000000000000000 ) ;
#4583 = VERTEX_POINT ( 'NONE', #7313 ) ;
#4584 = CARTESIAN_POINT ( 'NONE',  ( -73.53125000204838102, 55.00000000000000000, -25.81189881249999729 ) ) ;
#4585 = CARTESIAN_POINT ( 'NONE',  ( -32.72515708217407138, 34.82695427582095959, -6.127117481167428714 ) ) ;
#4586 = PRESENTATION_STYLE_ASSIGNMENT (( #10080 ) ) ;
#4587 = ORIENTED_EDGE ( 'NONE', *, *, #140, .F. ) ;
#4588 = FACE_OUTER_BOUND ( 'NONE', #10612, .T. ) ;
#4589 = CARTESIAN_POINT ( 'NONE',  ( -67.88985479635340425, 48.90596771384532815, 3.517032652760510913 ) ) ;
#4590 = ORIENTED_EDGE ( 'NONE', *, *, #2362, .T. ) ;
#4591 = CARTESIAN_POINT ( 'NONE',  ( -41.88142568112290576, 58.08538812386944983, -20.80148275009198855 ) ) ;
#4592 = CARTESIAN_POINT ( 'NONE',  ( 0.2748429140369315071, 38.70467982241823535, -13.38321124372595783 ) ) ;
#4593 = FACE_OUTER_BOUND ( 'NONE', #3501, .T. ) ;
#4594 = CYLINDRICAL_SURFACE ( 'NONE', #11352, 29.00000000000000355 ) ;
#4595 = DIRECTION ( 'NONE',  ( 0.000000000000000000, 0.000000000000000000, 1.000000000000000000 ) ) ;
#4596 = CARTESIAN_POINT ( 'NONE',  ( -2.500000000000005773, -4.330127018922191873, -6.099999999999999645 ) ) ;
#4597 = EDGE_LOOP ( 'NONE', ( #4290, #7413, #1314, #4304 ) ) ;
#4598 = CARTESIAN_POINT ( 'NONE',  ( -76.81250000000007105, 72.67766952966361771, -17.67766952966362126 ) ) ;
#4599 = CARTESIAN_POINT ( 'NONE',  ( -41.56959446453805640, 54.99645083705581072, -0.01182256036410916228 ) ) ;
#4600 = CARTESIAN_POINT ( 'NONE',  ( -57.45740457225677034, 55.65951194273775826, 4.966982812372184419 ) ) ;
#4601 = CONICAL_SURFACE ( 'NONE', #955, 5.000000000000000888, 1.047197551196596299 ) ;
#4602 = ADVANCED_FACE ( 'NONE', ( #10098 ), #7366, .T. ) ;
#4603 = DIRECTION ( 'NONE',  ( 0.000000000000000000, 0.000000000000000000, -1.000000000000000000 ) ) ;
#4604 = VECTOR ( 'NONE', #11137, 1000.000000000000000 ) ;
#4605 = DIRECTION ( 'NONE',  ( -1.000000000000000000, -0.000000000000000000, -0.000000000000000000 ) ) ;
#4606 = ORIENTED_EDGE ( 'NONE', *, *, #11689, .T. ) ;
#4607 = CARTESIAN_POINT ( 'NONE',  ( 17.18896242946999919, 60.50854855881860317, 20.47421955154796436 ) ) ;
#4608 = CIRCLE ( 'NONE', #965, 1.500000000000001332 ) ;
#4609 = CARTESIAN_POINT ( 'NONE',  ( -80.00000000000001421, 54.99999999999998579, -6.985278002320760571 ) ) ;
#4610 = CARTESIAN_POINT ( 'NONE',  ( 12.12266132830104226, 54.34318581670489579, 4.967339324998079064 ) ) ;
#4611 = CARTESIAN_POINT ( 'NONE',  ( -72.31250000204839523, 29.18810118750000626, -10.69163855873949309 ) ) ;
#4612 = CARTESIAN_POINT ( 'NONE',  ( -77.46875000204839523, 73.25176868561975141, 18.25176868561974075 ) ) ;
#4613 = EDGE_LOOP ( 'NONE', ( #6741, #11745, #8633, #1148 ) ) ;
#4614 = CARTESIAN_POINT ( 'NONE',  ( -77.84375000204839523, 55.00000000000000000, -25.81189881249999729 ) ) ;
#4615 = AXIS2_PLACEMENT_3D ( 'NONE', #10964, #9957, #6497 ) ;
#4616 = ORIENTED_EDGE ( 'NONE', *, *, #5340, .F. ) ;
#4617 = CARTESIAN_POINT ( 'NONE',  ( 5.544577452450643484, 50.12720890011707553, -1.300076040883277884 ) ) ;
#4618 = CARTESIAN_POINT ( 'NONE',  ( 4.335193296466895774, 42.05253176472596977, -5.362557364853363318 ) ) ;
#4619 = EDGE_CURVE ( 'NONE', #1706, #11337, #7882, .T. ) ;
#4620 = CARTESIAN_POINT ( 'NONE',  ( -76.81250000204839523, 29.18810118750000981, 10.69163855873950020 ) ) ;
#4621 = CYLINDRICAL_SURFACE ( 'NONE', #1474, 1.499999999999999556 ) ;
#4622 = CYLINDRICAL_SURFACE ( 'NONE', #10076, 20.00000000000000355 ) ;
#4623 = AXIS2_PLACEMENT_3D ( 'NONE', #9265, #5813, #2927 ) ;
#4624 = AXIS2_PLACEMENT_3D ( 'NONE', #7163, #2598, #9064 ) ;
#4625 = ORIENTED_EDGE ( 'NONE', *, *, #7410, .F. ) ;
#4626 = PRODUCT_DEFINITION_SHAPE ( 'NONE', 'NONE',  #11854 ) ;
#4627 = LINE ( 'NONE', #3553, #7837 ) ;
#4628 = CARTESIAN_POINT ( 'NONE',  ( -78.03125000409677625, 44.64466094067262958, 25.00000000000001066 ) ) ;
#4629 = ADVANCED_FACE ( 'NONE', ( #10941 ), #7142, .T. ) ;
#4630 = FACE_OUTER_BOUND ( 'NONE', #11394, .T. ) ;
#4631 = CARTESIAN_POINT ( 'NONE',  ( -28.53821618333067534, 54.99572319873755788, 0.001494283935380159292 ) ) ;
#4632 = SHAPE_DEFINITION_REPRESENTATION ( #3566, #11597 ) ;
#4633 = CARTESIAN_POINT ( 'NONE',  ( -19.45868386605759426, 75.13175751020747839, 8.896918319219480509 ) ) ;
#4634 = CARTESIAN_POINT ( 'NONE',  ( 0.000000000000000000, 0.000000000000000000, -4.346257142857142597 ) ) ;
#4635 = EDGE_CURVE ( 'NONE', #2349, #11145, #5784, .T. ) ;
#4636 = ORIENTED_EDGE ( 'NONE', *, *, #9664, .F. ) ;
#4637 = CARTESIAN_POINT ( 'NONE',  ( 7.485949637387768085, 50.00826809906988757, 0.3311691434445088178 ) ) ;
#4638 = CARTESIAN_POINT ( 'NONE',  ( -3.000000000000000000, 0.000000000000000000, -4.346257142857142597 ) ) ;
#4639 = ORIENTED_EDGE ( 'NONE', *, *, #4051, .F. ) ;
#4640 = CARTESIAN_POINT ( 'NONE',  ( 0.8268573817076104726, 37.44832105976551873, -11.71822709476406210 ) ) ;
#4641 = CARTESIAN_POINT ( 'NONE',  ( -77.75000000204839523, 65.69163855873948421, -25.81189881250000440 ) ) ;
#4642 = EDGE_LOOP ( 'NONE', ( #6275, #1003, #114, #770 ) ) ;
#4643 = CARTESIAN_POINT ( 'NONE',  ( -71.84375000204838102, 73.25176868561975141, -18.25176868561974430 ) ) ;
#4644 = CARTESIAN_POINT ( 'NONE',  ( -8.839809468419982608, 72.54364378520992318, -11.73195350307014273 ) ) ;
#4645 = DIRECTION ( 'NONE',  ( 0.000000000000000000, 1.000000000000000000, 0.000000000000000000 ) ) ;
#4646 = EDGE_LOOP ( 'NONE', ( #5603, #4105, #3176, #4859 ) ) ;
#4647 = CARTESIAN_POINT ( 'NONE',  ( -10.81689418260944180, 58.76766599462401786, -3.303253631844218940 ) ) ;
#4648 = CYLINDRICAL_SURFACE ( 'NONE', #4805, 25.00000000000000355 ) ;
#4649 = ORIENTED_EDGE ( 'NONE', *, *, #10875, .T. ) ;
#4650 = CARTESIAN_POINT ( 'NONE',  ( -52.36394100382401717, 74.78921131832989033, 7.080786878544920171 ) ) ;
#4651 = CARTESIAN_POINT ( 'NONE',  ( -5.608280846031337141, 57.05942937149918492, -21.01412426850803783 ) ) ;
#4652 = LINE ( 'NONE', #10033, #5085 ) ;
#4653 = CARTESIAN_POINT ( 'NONE',  ( 22.23809523809524435, 59.99999999999998579, 0.000000000000000000 ) ) ;
#4654 = CARTESIAN_POINT ( 'NONE',  ( -15.00000000000000355, 5.000000000000000000, 30.00000000000000711 ) ) ;
#4655 = VERTEX_POINT ( 'NONE', #2576 ) ;
#4656 = LINE ( 'NONE', #3699, #4425 ) ;
#4657 = CARTESIAN_POINT ( 'NONE',  ( -33.12853505168487089, 55.00369317299735172, 0.0002287014689915395241 ) ) ;
#4658 = CARTESIAN_POINT ( 'NONE',  ( -55.51934695731827674, 57.21273593182136352, 4.486748991334322589 ) ) ;
#4659 = DIRECTION ( 'NONE',  ( 1.000000000000000000, 0.000000000000000000, 0.000000000000000000 ) ) ;
#4660 = DIRECTION ( 'NONE',  ( 0.000000000000000000, 0.000000000000000000, -1.000000000000000000 ) ) ;
#4661 = CARTESIAN_POINT ( 'NONE',  ( -58.40439726469009685, 61.62069348438144800, 12.39615534886321235 ) ) ;
#4662 = VERTEX_POINT ( 'NONE', #10823 ) ;
#4663 = CARTESIAN_POINT ( 'NONE',  ( -6.214759040711413718, 65.81103152010582846, -18.03762937187994453 ) ) ;
#4664 = VECTOR ( 'NONE', #4183, 1000.000000000000000 ) ;
#4665 = CARTESIAN_POINT ( 'NONE',  ( -72.31250000204839523, 29.18810118750000626, -10.69163855873949132 ) ) ;
#4666 = DIRECTION ( 'NONE',  ( 0.000000000000000000, -0.000000000000000000, 1.000000000000000000 ) ) ;
#4667 = CARTESIAN_POINT ( 'NONE',  ( 3.571755578639977724, 50.00000000000001421, 2.874253840576960811E-12 ) ) ;
#4668 = CARTESIAN_POINT ( 'NONE',  ( -72.78125000204838102, 55.00000000000000000, 25.81189881249999729 ) ) ;
#4669 = CARTESIAN_POINT ( 'NONE',  ( -75.03125000204838102, 55.00000000000000000, -25.81189881249999729 ) ) ;
#4670 = VERTEX_POINT ( 'NONE', #3588 ) ;
#4671 = CARTESIAN_POINT ( 'NONE',  ( -78.21875000204839523, 29.18810118750000271, 4.741568889096522788E-15 ) ) ;
#4672 = ORIENTED_EDGE ( 'NONE', *, *, #10007, .F. ) ;
#4673 = CARTESIAN_POINT ( 'NONE',  ( 21.37139390916209436, 76.70668867414399017, -12.40776174393255005 ) ) ;
#4674 = CARTESIAN_POINT ( 'NONE',  ( -52.25615635136895776, 67.37056480795911284, 6.610292622630669079 ) ) ;
#4675 = EDGE_CURVE ( 'NONE', #6797, #7233, #9207, .T. ) ;
#4676 = ADVANCED_FACE ( 'NONE', ( #3940 ), #2143, .F. ) ;
#4677 = CARTESIAN_POINT ( 'NONE',  ( -77.93750000204838102, 44.30836144126049447, -25.81189881249999019 ) ) ;
#4678 = CARTESIAN_POINT ( 'NONE',  ( -75.00000000000000000, 80.04891742985661551, -3.510137850074999122 ) ) ;
#4679 = DIRECTION ( 'NONE',  ( -1.000000000000000000, 0.000000000000000000, 0.000000000000000000 ) ) ;
#4680 = ORIENTED_EDGE ( 'NONE', *, *, #4268, .F. ) ;
#4681 = CARTESIAN_POINT ( 'NONE',  ( -78.87500000000000000, 30.00000000000000355, 4.592425496802573578E-15 ) ) ;
#4682 = CARTESIAN_POINT ( 'NONE',  ( -72.40625000204839523, 36.74823131438026280, 18.25176868561974786 ) ) ;
#4683 = DIRECTION ( 'NONE',  ( 0.000000000000000000, 1.000000000000000000, 0.000000000000000000 ) ) ;
#4684 = FACE_BOUND ( 'NONE', #11330, .T. ) ;
#4685 = CARTESIAN_POINT ( 'NONE',  ( -56.23628154728545780, 55.00641776599200483, 0.01848975112542444732 ) ) ;
#4686 = SHAPE_DEFINITION_REPRESENTATION ( #8071, #4172 ) ;
#4687 = EDGE_CURVE ( 'NONE', #847, #7502, #10401, .T. ) ;
#4688 = AXIS2_PLACEMENT_3D ( 'NONE', #3102, #4840, #2190 ) ;
#4689 = CARTESIAN_POINT ( 'NONE',  ( -21.66859339435655230, 76.96133620317469592, -1.491344961900184174 ) ) ;
#4690 = EDGE_CURVE ( 'NONE', #8651, #5122, #5392, .T. ) ;
#4691 = EDGE_CURVE ( 'NONE', #3874, #66, #6594, .T. ) ;
#4692 = FACE_OUTER_BOUND ( 'NONE', #11736, .T. ) ;
#4693 = ORIENTED_EDGE ( 'NONE', *, *, #5576, .F. ) ;
#4694 = CARTESIAN_POINT ( 'NONE',  ( -75.00000000000000000, 55.00000000000000711, -29.00000000000000355 ) ) ;
#4695 = CARTESIAN_POINT ( 'NONE',  ( -73.71875000409679046, 65.35533905932720700, 25.00000000000016698 ) ) ;
#4696 = ORIENTED_EDGE ( 'NONE', *, *, #11196, .F. ) ;
#4697 = CARTESIAN_POINT ( 'NONE',  ( 14.47760468889531182, 57.74566952947367326, 20.98118467575540436 ) ) ;
#4698 =( BOUNDED_SURFACE ( )  B_SPLINE_SURFACE ( 1, 2, ( 
 ( #7060, #9730, #5309, #681, #8901, #9793, #1586, #5194, #8847, #6335, #4289, #11522, #8964, #4354, #6996, #11706, #7947, #1530, #7173, #625, #10797, #11581, #738, #5254, #3383, #10619, #2668, #10680, #2430, #2493, #4413, #6158, #8005, #3446, #7118, #9908, #10743, #6216, #8064, #9848, #10860, #1640, #2608, #3506, #9964, #11757, #4232, #1704, #5368, #9020, #4470, #8122, #3563, #7892, #7235, #5136, #8784, #565, #10202, #1812, #3798, #3735, #10920, #2732, #6390, #1995, #13, #5480, #2838, #3865, #9075, #5665, #9187, #8413, #3683, #10018, #4523, #7401, #8178, #851, #9129, #9302, #910, #6506, #5608, #71, #2782 ),
 ( #1096, #4581, #5425, #9247, #7526, #4760, #6629, #196, #8237, #7346, #10971, #1936, #976, #5541, #6444, #10074, #1873, #4641, #2963, #8293, #11817, #1035, #11029, #3622, #8349, #10135, #4699, #7468, #134, #11092, #2904, #6573, #11148, #1760, #7290, #7814, #6689, #254, #4825, #9549, #3919, #6753, #7584, #2117, #1344, #10320, #377, #10434, #11387, #3982, #5974, #11445, #11211, #1156, #10381, #4152, #2177, #3255, #317, #5845, #9486, #8711, #8657, #7641, #1276, #4043, #5794, #11271, #5064, #9610, #8478, #436, #5008, #4097, #4945, #3082, #2298, #9426, #495, #6806, #3022, #8533, #6868, #1216, #10259, #7699, #8601 ) ),
 .UNSPECIFIED., .F., .F., .T. ) 
 B_SPLINE_SURFACE_WITH_KNOTS ( ( 2, 2 ),
 ( 3, 2, 2, 2, 2, 2, 2, 2, 2, 2, 2, 2, 2, 2, 2, 2, 2, 2, 2, 2, 2, 2, 2, 2, 2, 2, 2, 2, 2, 2, 2, 2, 2, 2, 2, 2, 2, 2, 2, 2, 2, 2, 2, 3 ),
 ( 0.000000000000000000, 1.000000000000000000 ),
 ( 0.000000000000000000, 0.02083333333333333218, 0.04166666666666666435, 0.06250000000000000000, 0.08333333333333332871, 0.1041666666666666713, 0.1250000000000000000, 0.1458333333333333426, 0.1666666666666666574, 0.1875000000000000000, 0.2083333333333333426, 0.2291666666666666574, 0.2500000000000000000, 0.2708333333333333148, 0.2916666666666666852, 0.3125000000000000000, 0.3333333333333333148, 0.3541666666666666852, 0.3750000000000000000, 0.3958333333333333148, 0.4166666666666666852, 0.4375000000000000000, 0.4583333333333333148, 0.4791666666666666852, 0.5000000000000000000, 0.5208333333333333703, 0.5416666666666666297, 0.5625000000000000000, 0.5833333333333333703, 0.6041666666666666297, 0.6250000000000000000, 0.6458333333333333703, 0.6666666666666666297, 0.6875000000000000000, 0.7083333333333333703, 0.7291666666666666297, 0.7500000000000000000, 0.7708333333333333703, 0.7916666666666666297, 0.8125000000000000000, 0.8333333333333333703, 0.8541666666666666297, 0.8750000000000000000, 0.8888490476107191451 ),
 .UNSPECIFIED. ) 
 GEOMETRIC_REPRESENTATION_ITEM ( )  RATIONAL_B_SPLINE_SURFACE ( (
 ( 1.000000000000000000, 0.9238795325112867385, 1.000000000000000000, 0.9238795325112867385, 1.000000000000000000, 0.9238795325112867385, 1.000000000000000000, 0.9238795325112867385, 1.000000000000000000, 0.9238795325112867385, 1.000000000000000000, 0.9238795325112867385, 1.000000000000000000, 0.9238795325112867385, 1.000000000000000000, 0.9238795325112867385, 1.000000000000000000, 0.9238795325112867385, 1.000000000000000000, 0.9238795325112867385, 1.000000000000000000, 0.9238795325112867385, 1.000000000000000000, 0.9238795325112867385, 1.000000000000000000, 0.9238795325112867385, 1.000000000000000000, 0.9238795325112867385, 1.000000000000000000, 0.9238795325112867385, 1.000000000000000000, 0.9238795325112867385, 1.000000000000000000, 0.9238795325112867385, 1.000000000000000000, 0.9238795325112867385, 1.000000000000000000, 0.9238795325112867385, 1.000000000000000000, 0.9238795325112867385, 1.000000000000000000, 0.9238795325112867385, 1.000000000000000000, 0.9238795325112867385, 1.000000000000000000, 0.9238795325112867385, 1.000000000000000000, 0.9238795325112867385, 1.000000000000000000, 0.9238795325112867385, 1.000000000000000000, 0.9238795325112867385, 1.000000000000000000, 0.9238795325112867385, 1.000000000000000000, 0.9238795325112867385, 1.000000000000000000, 0.9238795325112867385, 1.000000000000000000, 0.9238795325112867385, 1.000000000000000000, 0.9238795325112867385, 1.000000000000000000, 0.9238795325112867385, 1.000000000000000000, 0.9238795325112867385, 1.000000000000000000, 0.9238795325112867385, 1.000000000000000000, 0.9238795325112867385, 1.000000000000000000, 0.9238795325112867385, 1.000000000000000000, 0.9238795325112867385, 1.000000000000000000, 0.9238795325112867385, 1.000000000000000000, 0.9238795325112867385, 1.000000000000000000, 0.9238795325112867385, 1.000000000000000000, 0.9238795325112867385, 1.000000000000000000, 0.9238795325112867385, 1.000000000000000000, 0.9493985930367334625, 0.9660721903170175207),
 ( 1.000000000000000000, 0.9238795325112867385, 1.000000000000000000, 0.9238795325112867385, 1.000000000000000000, 0.9238795325112867385, 1.000000000000000000, 0.9238795325112867385, 1.000000000000000000, 0.9238795325112867385, 1.000000000000000000, 0.9238795325112867385, 1.000000000000000000, 0.9238795325112867385, 1.000000000000000000, 0.9238795325112867385, 1.000000000000000000, 0.9238795325112867385, 1.000000000000000000, 0.9238795325112867385, 1.000000000000000000, 0.9238795325112867385, 1.000000000000000000, 0.9238795325112867385, 1.000000000000000000, 0.9238795325112867385, 1.000000000000000000, 0.9238795325112867385, 1.000000000000000000, 0.9238795325112867385, 1.000000000000000000, 0.9238795325112867385, 1.000000000000000000, 0.9238795325112867385, 1.000000000000000000, 0.9238795325112867385, 1.000000000000000000, 0.9238795325112867385, 1.000000000000000000, 0.9238795325112867385, 1.000000000000000000, 0.9238795325112867385, 1.000000000000000000, 0.9238795325112867385, 1.000000000000000000, 0.9238795325112867385, 1.000000000000000000, 0.9238795325112867385, 1.000000000000000000, 0.9238795325112867385, 1.000000000000000000, 0.9238795325112867385, 1.000000000000000000, 0.9238795325112867385, 1.000000000000000000, 0.9238795325112867385, 1.000000000000000000, 0.9238795325112867385, 1.000000000000000000, 0.9238795325112867385, 1.000000000000000000, 0.9238795325112867385, 1.000000000000000000, 0.9238795325112867385, 1.000000000000000000, 0.9238795325112867385, 1.000000000000000000, 0.9238795325112867385, 1.000000000000000000, 0.9238795325112867385, 1.000000000000000000, 0.9238795325112867385, 1.000000000000000000, 0.9238795325112867385, 1.000000000000000000, 0.9238795325112867385, 1.000000000000000000, 0.9238795325112867385, 1.000000000000000000, 0.9238795325112867385, 1.000000000000000000, 0.9238795325112867385, 1.000000000000000000, 0.9238795325112867385, 1.000000000000000000, 0.9493985930367334625, 0.9660721903170175207) ) ) 
 REPRESENTATION_ITEM ( '' )  SURFACE ( )  );
#4699 = CARTESIAN_POINT ( 'NONE',  ( -76.90625000204839523, 36.74823131438026280, 18.25176868561974786 ) ) ;
#4700 = EDGE_CURVE ( 'NONE', #4769, #3987, #11233, .T. ) ;
#4701 = EDGE_CURVE ( 'NONE', #4778, #11556, #10358, .T. ) ;
#4702 = EDGE_CURVE ( 'NONE', #10425, #9224, #9449, .T. ) ;
#4703 = CARTESIAN_POINT ( 'NONE',  ( 4.999999999999998224, -2.886751345948137981, -0.4465819873852071575 ) ) ;
#4704 = CARTESIAN_POINT ( 'NONE',  ( -36.47762819585614835, 42.07544065584382764, -16.80749884933775462 ) ) ;
#4705 = CARTESIAN_POINT ( 'NONE',  ( -56.05785376386896246, 64.93131079446247611, 18.59685268580366468 ) ) ;
#4706 = ORIENTED_EDGE ( 'NONE', *, *, #8065, .F. ) ;
#4707 = CARTESIAN_POINT ( 'NONE',  ( -71.46875000204838102, 80.81189881250000440, -1.580522963032174394E-15 ) ) ;
#4708 = CARTESIAN_POINT ( 'NONE',  ( 0.4609857007025546793, 50.66760339081043441, -2.501461926089155074 ) ) ;
#4709 = CARTESIAN_POINT ( 'NONE',  ( 8.189038476963473201, 38.19597440261895827, 12.92108669627241646 ) ) ;
#4710 = VECTOR ( 'NONE', #1487, 1000.000000000000000 ) ;
#4711 = EDGE_LOOP ( 'NONE', ( #4507, #11727, #4590, #8325 ) ) ;
#4712 = CARTESIAN_POINT ( 'NONE',  ( -47.18905769862622890, 73.33034157825031230, -10.56456148164999398 ) ) ;
#4713 = CARTESIAN_POINT ( 'NONE',  ( -64.51030549024622474, 43.28227691760346119, 17.55408017169854418 ) ) ;
#4714 = LINE ( 'NONE', #2743, #5873 ) ;
#4715 = AXIS2_PLACEMENT_3D ( 'NONE', #11085, #3912, #7578 ) ;
#4716 = DIRECTION ( 'NONE',  ( -1.000000000000000000, -0.000000000000000000, -0.000000000000000000 ) ) ;
#4717 = CARTESIAN_POINT ( 'NONE',  ( 39.99999999999999289, 55.00000000000000000, 0.000000000000000000 ) ) ;
#4718 = EDGE_LOOP ( 'NONE', ( #3774, #5748, #985 ) ) ;
#4719 = CARTESIAN_POINT ( 'NONE',  ( -79.90625000000000000, 65.35533905932737753, -24.99999999999999645 ) ) ;
#4720 = CARTESIAN_POINT ( 'NONE',  ( -21.46186838525607499, 54.99879797654112679, -0.003499567500229079815 ) ) ;
#4721 = CARTESIAN_POINT ( 'NONE',  ( -45.79623854691614326, 59.33124940395137514, -2.503488177144706395 ) ) ;
#4722 = CARTESIAN_POINT ( 'NONE',  ( -15.00000000000000355, 5.000000000000000000, -29.99999999999999289 ) ) ;
#4723 = AXIS2_PLACEMENT_3D ( 'NONE', #650, #4491, #7200 ) ;
#4724 = CARTESIAN_POINT ( 'NONE',  ( 6.123233995736763324E-16, -57.00000000000000000, 4.999999999999997335 ) ) ;
#4725 = CARTESIAN_POINT ( 'NONE',  ( 22.33333333333333570, 61.99999999999997868, 0.000000000000000000 ) ) ;
#4726 = AXIS2_PLACEMENT_3D ( 'NONE', #9336, #1192, #2874 ) ;
#4727 = ORIENTED_EDGE ( 'NONE', *, *, #11418, .T. ) ;
#4728 = CARTESIAN_POINT ( 'NONE',  ( -78.00000000000001421, 54.99999999999999289, -15.47055937655931501 ) ) ;
#4729 = FACE_OUTER_BOUND ( 'NONE', #4613, .T. ) ;
#4730 = CYLINDRICAL_SURFACE ( 'NONE', #9759, 24.99999999999999645 ) ;
#4731 = CARTESIAN_POINT ( 'NONE',  ( 0.000000000000000000, 0.000000000000000000, -5.210428571428570521 ) ) ;
#4732 = CARTESIAN_POINT ( 'NONE',  ( -73.15625000204838102, 80.81189881250000440, -1.580522963032174394E-15 ) ) ;
#4733 = CARTESIAN_POINT ( 'NONE',  ( -72.59375000204838102, 36.74823131438026280, 18.25176868561974786 ) ) ;
#4734 = ORIENTED_EDGE ( 'NONE', *, *, #3812, .F. ) ;
#4735 = CARTESIAN_POINT ( 'NONE',  ( -78.50000000204840944, 44.30836144126053000, 25.81189881250000795 ) ) ;
#4736 = ORIENTED_EDGE ( 'NONE', *, *, #10695, .F. ) ;
#4737 =( NAMED_UNIT ( * ) PLANE_ANGLE_UNIT ( ) SI_UNIT ( $, .RADIAN. ) );
#4738 = AXIS2_PLACEMENT_3D ( 'NONE', #6164, #8011, #1383 ) ;
#4739 = CARTESIAN_POINT ( 'NONE',  ( -41.45530645628071653, 58.40375168898731317, -13.59199727772139710 ) ) ;
#4740 = MANIFOLD_SOLID_BREP ( 'M10 Machine Threads Stud1', #416 ) ;
#4741 = DIRECTION ( 'NONE',  ( 1.000000000000000000, 0.000000000000000000, 0.000000000000000000 ) ) ;
#4742 = EDGE_CURVE ( 'NONE', #7798, #10526, #1299, .T. ) ;
#4743 = CARTESIAN_POINT ( 'NONE',  ( -74.99999999999998579, 79.48388272459020243, -6.547252175383230899 ) ) ;
#4744 = PLANE ( 'NONE',  #2453 ) ;
#4745 = AXIS2_PLACEMENT_3D ( 'NONE', #8396, #4806, #3780 ) ;
#4746 = VERTEX_POINT ( 'NONE', #5752 ) ;
#4747 = CARTESIAN_POINT ( 'NONE',  ( -80.00000000000001421, 59.24264068711927678, 4.242644059037073312 ) ) ;
#4748 = CARTESIAN_POINT ( 'NONE',  ( -76.34375000409680467, 30.00000000000001421, 10.35533905932739174 ) ) ;
#4749 = CARTESIAN_POINT ( 'NONE',  ( -34.15346748487235828, 50.00825927070384580, -0.3308703489901499428 ) ) ;
#4750 = FACE_BOUND ( 'NONE', #3380, .T. ) ;
#4751 = CARTESIAN_POINT ( 'NONE',  ( 4.375386355529371052, 48.65700148509509404, -3.000201103635157018 ) ) ;
#4752 = VECTOR ( 'NONE', #9099, 1000.000000000000000 ) ;
#4753 = CARTESIAN_POINT ( 'NONE',  ( -80.00000000000001421, 59.24264068711927678, 4.242644059037073312 ) ) ;
#4754 = CARTESIAN_POINT ( 'NONE',  ( -15.00000000000000000, -24.99999999999999645, 10.00000000000000000 ) ) ;
#4755 = ORIENTED_EDGE ( 'NONE', *, *, #4012, .F. ) ;
#4756 = PLANE ( 'NONE',  #7042 ) ;
#4757 = DIRECTION ( 'NONE',  ( -1.000000000000000000, -0.000000000000000000, -0.000000000000000000 ) ) ;
#4758 = ORIENTED_EDGE ( 'NONE', *, *, #2480, .T. ) ;
#4759 = CARTESIAN_POINT ( 'NONE',  ( -9.662811212962280294, 69.86524355530642083, -14.86597185903763219 ) ) ;
#4760 = CARTESIAN_POINT ( 'NONE',  ( -78.87500000204838102, 80.81189881250001861, 10.69163855873948599 ) ) ;
#4761 = CARTESIAN_POINT ( 'NONE',  ( -15.00000000000000000, -30.00000000000000000, 10.00000000000000000 ) ) ;
#4762 = CARTESIAN_POINT ( 'NONE',  ( -43.83980969374544401, 66.71858909844225138, -17.55257377017560216 ) ) ;
#4763 = CARTESIAN_POINT ( 'NONE',  ( -51.69727455458300369, 74.78870212167194609, 7.080596778485133136 ) ) ;
#4764 = ORIENTED_EDGE ( 'NONE', *, *, #869, .T. ) ;
#4765 = CARTESIAN_POINT ( 'NONE',  ( -72.96875000204838102, 80.81189881250000440, -1.580522963032174394E-15 ) ) ;
#4766 = EDGE_CURVE ( 'NONE', #3266, #1626, #8556, .T. ) ;
#4767 = CARTESIAN_POINT ( 'NONE',  ( -3.044769863957841327, 52.78589301970062309, -4.495079137651556422 ) ) ;
#4768 = CARTESIAN_POINT ( 'NONE',  ( 5.506399570602333426, 34.30736306936326230, 4.109392375493936100 ) ) ;
#4769 = VERTEX_POINT ( 'NONE', #93 ) ;
#4770 = CARTESIAN_POINT ( 'NONE',  ( -43.63602718628743560, 63.99223089048333435, -19.01333957068342428 ) ) ;
#4771 = CARTESIAN_POINT ( 'NONE',  ( -58.05785365788000263, 64.93276152744238061, 18.60033633024681521 ) ) ;
#4772 = CARTESIAN_POINT ( 'NONE',  ( -78.00000000000001421, 46.51471862576140381, -8.485278002320759683 ) ) ;
#4773 = CARTESIAN_POINT ( 'NONE',  ( -80.00000000000002842, 42.27207793864211283, 12.72792543327562775 ) ) ;
#4774 = AXIS2_PLACEMENT_3D ( 'NONE', #9039, #5271, #10760 ) ;
#4775 = CARTESIAN_POINT ( 'NONE',  ( 0.000000000000000000, 0.000000000000000000, -3.832189483390572970 ) ) ;
#4776 = CARTESIAN_POINT ( 'NONE',  ( -75.21875000409676204, 65.35533905932724963, 25.00000000000012434 ) ) ;
#4777 = EDGE_CURVE ( 'NONE', #7952, #10233, #7428, .T. ) ;
#4778 = VERTEX_POINT ( 'NONE', #10163 ) ;
#4779 = CARTESIAN_POINT ( 'NONE',  ( -76.53124999999998579, 80.00000000000001421, 10.35533905932737397 ) ) ;
#4780 = CARTESIAN_POINT ( 'NONE',  ( -22.33546444871533154, 54.99950364521073709, -0.001766467382170159531 ) ) ;
#4781 = CARTESIAN_POINT ( 'NONE',  ( -48.90475262238859244, 59.99999999999997158, -9.564595459368971197E-12 ) ) ;
#4782 = B_SPLINE_CURVE_WITH_KNOTS ( 'NONE', 3,
 ( #834, #6260, #10003, #10723 ),
 .UNSPECIFIED., .F., .F.,
 ( 4, 4 ),
 ( 2.380735200850351173E-07, 0.002921158011986708155 ),
 .UNSPECIFIED. ) ;
#4783 = CARTESIAN_POINT ( 'NONE',  ( -3.000000000000000000, 0.000000000000000000, -0.8895714285714284575 ) ) ;
#4784 = AXIS2_PLACEMENT_3D ( 'NONE', #4383, #7029, #10772 ) ;
#4785 = FACE_OUTER_BOUND ( 'NONE', #2833, .T. ) ;
#4786 = CARTESIAN_POINT ( 'NONE',  ( -59.59524304407526074, 59.09388748838112093, 13.47225211819516666 ) ) ;
#4787 = ORIENTED_EDGE ( 'NONE', *, *, #9382, .T. ) ;
#4788 = CARTESIAN_POINT ( 'NONE',  ( -3.608280849245335542, 57.05942974268126022, -21.01780866629736977 ) ) ;
#4789 = UNCERTAINTY_MEASURE_WITH_UNIT (LENGTH_MEASURE( 1.000000000000000082E-05 ), #10005, 'distance_accuracy_value', 'NONE');
#4790 = DIRECTION ( 'NONE',  ( 0.000000000000000000, 1.000000000000000000, 0.000000000000000000 ) ) ;
#4791 = CYLINDRICAL_SURFACE ( 'NONE', #1022, 2.999999999999999112 ) ;
#4793 = B_SPLINE_CURVE_WITH_KNOTS ( 'NONE', 3,
 ( #4312, #6243, #9933, #11782, #10708, #7257, #6360, #5336, #4550, #8202, #9043, #1556, #2522, #2633, #4439, #820, #1667, #3411, #8143, #10826, #9988, #3349, #6187, #3590, #5222, #8870, #10884, #7971, #11607, #8925, #2695, #1782, #5449, #7022 ),
 .UNSPECIFIED., .F., .F.,
 ( 4, 2, 2, 2, 2, 2, 2, 2, 2, 2, 2, 2, 2, 2, 2, 2, 4 ),
 ( 0.09713928911131490540, 0.09865623822481217609, 0.1001731873383094468, 0.1016901364518067175, 0.1032070855653039881, 0.1047240346788012588, 0.1062409837922985295, 0.1077579329057958002, 0.1092748820192930709, 0.1107918311327903138, 0.1123087802462875706, 0.1138257293597848274, 0.1153426784732820842, 0.1168596275867793410, 0.1183765767002765978, 0.1198935258137738408, 0.1214104749272710976 ),
 .UNSPECIFIED. ) ;
#4792 = FACE_OUTER_BOUND ( 'NONE', #1931, .T. ) ;
#4794 = CARTESIAN_POINT ( 'NONE',  ( -0.8657091724475090011, 65.44905221436334841, -22.71165102530780899 ) ) ;
#4795 = CARTESIAN_POINT ( 'NONE',  ( -73.15625000204838102, 80.81189881250000440, -1.580522963032174394E-15 ) ) ;
#4796 = ORIENTED_EDGE ( 'NONE', *, *, #7193, .F. ) ;
#4797 = CARTESIAN_POINT ( 'NONE',  ( -71.46875000204838102, 80.81189881250000440, -1.580522963032174394E-15 ) ) ;
#4798 = ORIENTED_EDGE ( 'NONE', *, *, #7702, .F. ) ;
#4799 = CARTESIAN_POINT ( 'NONE',  ( 16.14987959356399472, 72.61399012904941230, -17.75150298415823258 ) ) ;
#4800 = CARTESIAN_POINT ( 'NONE',  ( -39.70300543809604221, 54.31243699202812536, -13.99175817854623816 ) ) ;
#4801 = AXIS2_PLACEMENT_3D ( 'NONE', #119, #11807, #3671 ) ;
#4802 = CARTESIAN_POINT ( 'NONE',  ( -79.15625000204838102, 80.81189881250000440, -1.580522963032174394E-15 ) ) ;
#4803 = EDGE_CURVE ( 'NONE', #8948, #1817, #1960, .T. ) ;
#4804 = CARTESIAN_POINT ( 'NONE',  ( -74.99999999999998579, 74.03124084216746326, -17.00900853765869059 ) ) ;
#4805 = AXIS2_PLACEMENT_3D ( 'NONE', #2067, #8423, #2128 ) ;
#4806 = DIRECTION ( 'NONE',  ( -1.000000000000000000, -0.000000000000000000, -0.000000000000000000 ) ) ;
#4807 = ORIENTED_EDGE ( 'NONE', *, *, #5783, .F. ) ;
#4808 = AXIS2_PLACEMENT_3D ( 'NONE', #5231, #8878, #7094 ) ;
#4809 = VECTOR ( 'NONE', #11682, 1000.000000000000000 ) ;
#4810 = CARTESIAN_POINT ( 'NONE',  ( -71.84302369010728739, 76.88501343918500197, 12.63531067400213104 ) ) ;
#4811 = DIRECTION ( 'NONE',  ( 0.000000000000000000, 0.000000000000000000, 1.000000000000000000 ) ) ;
#4812 = DIRECTION ( 'NONE',  ( -1.000000000000000000, -6.033820786006286457E-17, 0.000000000000000000 ) ) ;
#4813 = DIRECTION ( 'NONE',  ( 0.000000000000000000, 1.000000000000000000, 0.000000000000000000 ) ) ;
#4814 = CARTESIAN_POINT ( 'NONE',  ( -17.79192078018706624, 58.60112408783383131, 6.006281318062062446 ) ) ;
#4815 = CARTESIAN_POINT ( 'NONE',  ( 62.44550000000000267, 55.00000000000000000, 2.999999999999995559 ) ) ;
#4816 = AXIS2_PLACEMENT_3D ( 'NONE', #1236, #3043, #7547 ) ;
#4817 = DIRECTION ( 'NONE',  ( -1.000000000000000000, -0.000000000000000000, -0.000000000000000000 ) ) ;
#4818 = VECTOR ( 'NONE', #6969, 1000.000000000000000 ) ;
#4819 = EDGE_LOOP ( 'NONE', ( #9284, #7998 ) ) ;
#4820 = ADVANCED_FACE ( 'NONE', ( #8498 ), #278, .F. ) ;
#4821 = DIRECTION ( 'NONE',  ( 1.000000000000000000, 0.000000000000000000, 0.000000000000000000 ) ) ;
#4822 = DIRECTION ( 'NONE',  ( -1.000000000000000000, -0.000000000000000000, -0.000000000000000000 ) ) ;
#4823 = ORIENTED_EDGE ( 'NONE', *, *, #1557, .T. ) ;
#4824 = CARTESIAN_POINT ( 'NONE',  ( -56.63607177307330431, 69.12418599258134577, 15.58301102096070245 ) ) ;
#4825 = CARTESIAN_POINT ( 'NONE',  ( -75.78125000204839523, 73.25176868561975141, 18.25176868561974075 ) ) ;
#4826 = EDGE_CURVE ( 'NONE', #11373, #10439, #400, .T. ) ;
#4827 = CIRCLE ( 'NONE', #9191, 1.500000000000001332 ) ;
#4828 = LINE ( 'NONE', #1996, #4435 ) ;
#4829 = DIRECTION ( 'NONE',  ( -1.000000000000000000, -0.000000000000000000, -0.000000000000000000 ) ) ;
#4830 = FACE_OUTER_BOUND ( 'NONE', #6926, .T. ) ;
#4831 = ORIENTED_EDGE ( 'NONE', *, *, #3960, .T. ) ;
#4832 = FACE_OUTER_BOUND ( 'NONE', #3329, .T. ) ;
#4833 = ADVANCED_FACE ( 'NONE', ( #9737 ), #513, .F. ) ;
#4834 = CARTESIAN_POINT ( 'NONE',  ( -9.069501975036009966, 57.64327492203570102, -4.247356385754962105 ) ) ;
#4835 = DIRECTION ( 'NONE',  ( -1.000000000000000000, -0.000000000000000000, -0.000000000000000000 ) ) ;
#4836 = VERTEX_POINT ( 'NONE', #5993 ) ;
#4837 = CARTESIAN_POINT ( 'NONE',  ( -51.49358338236809374, 75.68949746983442139, 4.121906040642151936 ) ) ;
#4838 = CARTESIAN_POINT ( 'NONE',  ( 19.53960773325150768, 67.25030761837875559, 7.055968998884240229 ) ) ;
#4839 = CARTESIAN_POINT ( 'NONE',  ( -80.00000000000001421, 63.48528137423857487, -8.485278002320759683 ) ) ;
#4840 = DIRECTION ( 'NONE',  ( -1.000000000000000000, -0.000000000000000000, -0.000000000000000000 ) ) ;
#4841 = DIRECTION ( 'NONE',  ( -1.000000000000000000, -0.000000000000000000, -0.000000000000000000 ) ) ;
#4842 = CARTESIAN_POINT ( 'NONE',  ( -72.12500000000007105, 79.99999999999987210, -1.530808498934183830E-15 ) ) ;
#4843 = ADVANCED_FACE ( 'NONE', ( #2256 ), #9798, .F. ) ;
#4844 = EDGE_LOOP ( 'NONE', ( #6921, #1400 ) ) ;
#4845 = CARTESIAN_POINT ( 'NONE',  ( -77.09374999999998579, 44.64466094067260826, -24.99999999999998934 ) ) ;
#4846 = CARTESIAN_POINT ( 'NONE',  ( -60.83651074932581082, 55.00008616263955474, -0.003570840406533045113 ) ) ;
#4847 = CARTESIAN_POINT ( 'NONE',  ( -7.511572993685809947E-16, -5.773502691896268857, -6.099999999999999645 ) ) ;
#4848 = ADVANCED_FACE ( 'NONE', ( #4965 ), #5030, .T. ) ;
#4849 = DIRECTION ( 'NONE',  ( 0.000000000000000000, 0.000000000000000000, -1.000000000000000000 ) ) ;
#4850 = ADVANCED_FACE ( 'NONE', ( #1365 ), #4175, .F. ) ;
#4851 = CARTESIAN_POINT ( 'NONE',  ( 2.208079232538515679, 48.20508033090954569, -1.701303895902414709 ) ) ;
#4852 = EDGE_LOOP ( 'NONE', ( #1455, #9924, #5836, #11754 ) ) ;
#4853 = CARTESIAN_POINT ( 'NONE',  ( -5.030643890195627854, 62.08057558410310861, -19.78873666113293694 ) ) ;
#4854 = LINE ( 'NONE', #7497, #11295 ) ;
#4855 = DIRECTION ( 'NONE',  ( 1.000000000000000000, 0.000000000000000000, 0.000000000000000000 ) ) ;
#4856 = PLANE ( 'NONE',  #11216 ) ;
#4857 = CARTESIAN_POINT ( 'NONE',  ( -22.24057001764307984, 77.42300265451373775, 11.08010208964972954 ) ) ;
#4858 = CARTESIAN_POINT ( 'NONE',  ( -77.84375000204839523, 55.00000000000000000, -25.81189881249999729 ) ) ;
#4859 = ORIENTED_EDGE ( 'NONE', *, *, #11249, .T. ) ;
#4860 = CARTESIAN_POINT ( 'NONE',  ( -73.15625000204839523, 73.25176868561975141, -18.25176868561974430 ) ) ;
#4861 = FACE_BOUND ( 'NONE', #959, .T. ) ;
#4862 = CARTESIAN_POINT ( 'NONE',  ( 18.44309544900626463, 74.35063009805416812, -15.88073011970089432 ) ) ;
#4863 = EDGE_CURVE ( 'NONE', #2849, #89, #10871, .T. ) ;
#4864 = CARTESIAN_POINT ( 'NONE',  ( 23.47754340821147068, 75.43020022661498558, 5.490793176664390707 ) ) ;
#4865 = CARTESIAN_POINT ( 'NONE',  ( 0.000000000000000000, 0.000000000000000000, -5.724496230895143256 ) ) ;
#4866 = PLANE ( 'NONE',  #7979 ) ;
#4867 = DIRECTION ( 'NONE',  ( 0.000000000000000000, 1.000000000000000000, 0.000000000000000000 ) ) ;
#4868 = ORIENTED_EDGE ( 'NONE', *, *, #3567, .F. ) ;
#4869 = CARTESIAN_POINT ( 'NONE',  ( -73.43750000000000000, 72.67766952966368876, 17.67766952966368521 ) ) ;
#4870 = CARTESIAN_POINT ( 'NONE',  ( -73.15625000409677625, 30.00000000000000355, -10.35533905932738108 ) ) ;
#4871 = CARTESIAN_POINT ( 'NONE',  ( -78.00000000000002842, 38.02943725152282184, 1.500003371917797867 ) ) ;
#4872 = AXIS2_PLACEMENT_3D ( 'NONE', #8860, #6231, #9691 ) ;
#4873 = ORIENTED_EDGE ( 'NONE', *, *, #8355, .F. ) ;
#4874 = CARTESIAN_POINT ( 'NONE',  ( 10.10998770594448359, 48.90696675832015927, 3.515728384091711511 ) ) ;
#4875 = DIRECTION ( 'NONE',  ( -1.000000000000000000, -0.000000000000000000, -0.000000000000000000 ) ) ;
#4876 = DIRECTION ( 'NONE',  ( 1.000000000000000000, 0.000000000000000000, 0.000000000000000000 ) ) ;
#4877 = ORIENTED_EDGE ( 'NONE', *, *, #10174, .F. ) ;
#4878 = DIRECTION ( 'NONE',  ( 0.000000000000000000, 0.000000000000000000, -1.000000000000000000 ) ) ;
#4879 = CARTESIAN_POINT ( 'NONE',  ( -78.50000000204842365, 29.18810118750000981, 10.69163855873950020 ) ) ;
#4880 = VERTEX_POINT ( 'NONE', #7836 ) ;
#4881 = CARTESIAN_POINT ( 'NONE',  ( -62.73530513678402087, 48.89572068339310107, 20.11073150603193938 ) ) ;
#4882 = DIRECTION ( 'NONE',  ( -0.7071067811865519026, 0.000000000000000000, 0.7071067811865431318 ) ) ;
#4883 = AXIS2_PLACEMENT_3D ( 'NONE', #9900, #555, #5183 ) ;
#4884 = CARTESIAN_POINT ( 'NONE',  ( 5.000000000000000000, 1.947085426416880649, -0.1996207071196908767 ) ) ;
#4885 = CARTESIAN_POINT ( 'NONE',  ( -79.34375000204839523, 55.00000000000000000, -25.81189881249999729 ) ) ;
#4886 = CARTESIAN_POINT ( 'NONE',  ( -77.84375000409677625, 30.00000000000001421, 10.35533905932739174 ) ) ;
#4887 = ORIENTED_EDGE ( 'NONE', *, *, #6623, .F. ) ;
#4888 = CARTESIAN_POINT ( 'NONE',  ( -78.00000000000002842, 38.02943725152282184, 3.371917797929946392E-06 ) ) ;
#4889 = CARTESIAN_POINT ( 'NONE',  ( 2.013601557404307574, 50.16004720627262969, -1.296442066224429146 ) ) ;
#4890 = EDGE_CURVE ( 'NONE', #7763, #6131, #8215, .T. ) ;
#4891 = CARTESIAN_POINT ( 'NONE',  ( 47.00000000000000000, 60.00000000000000000, 6.123233995736769241E-16 ) ) ;
#4892 = VERTEX_POINT ( 'NONE', #5201 ) ;
#4893 = CARTESIAN_POINT ( 'NONE',  ( 20.52241600750495820, 73.36972880021862409, 10.58068053353214566 ) ) ;
#4894 = CARTESIAN_POINT ( 'NONE',  ( 5.169754736345680612, 41.20621168070887563, 2.739677827818288947 ) ) ;
#4895 = LINE ( 'NONE', #3101, #8810 ) ;
#4896 = CARTESIAN_POINT ( 'NONE',  ( -77.37500000409677625, 55.00000000000000000, -24.99999999999999645 ) ) ;
#4897 = MANIFOLD_SOLID_BREP ( 'ThdSchPat', #5593 ) ;
#4898 = CARTESIAN_POINT ( 'NONE',  ( -19.37797842336306431, 58.76497942189116941, 3.306305682627446618 ) ) ;
#4899 = CARTESIAN_POINT ( 'NONE',  ( -75.78125000409680467, 65.35533905932749121, -24.99999999999989342 ) ) ;
#4900 = ADVANCED_FACE ( 'NONE', ( #11353 ), #1480, .T. ) ;
#4901 = ORIENTED_EDGE ( 'NONE', *, *, #8771, .T. ) ;
#4902 = CARTESIAN_POINT ( 'NONE',  ( -77.28124999999998579, 30.00000000000000355, -10.35533905932738108 ) ) ;
#4903 = CARTESIAN_POINT ( 'NONE',  ( -74.99999999999997158, 50.05679712599850006, -25.38984111367952679 ) ) ;
#4904 = EDGE_CURVE ( 'NONE', #8530, #7093, #2844, .T. ) ;
#4905 = CARTESIAN_POINT ( 'NONE',  ( -77.28125000000004263, 30.00000000000009948, -10.35533905932734378 ) ) ;
#4906 = AXIS2_PLACEMENT_3D ( 'NONE', #441, #8536, #2179 ) ;
#4907 = CARTESIAN_POINT ( 'NONE',  ( -80.00000000000002842, 46.51471862576140381, 8.485284746156354529 ) ) ;
#4908 = CARTESIAN_POINT ( 'NONE',  ( 7.556752435464094475, 49.39015905361354442, 4.313964523666476758 ) ) ;
#4909 = ORIENTED_EDGE ( 'NONE', *, *, #2765, .T. ) ;
#4910 = CARTESIAN_POINT ( 'NONE',  ( -34.85572910849313644, 38.22605186251247744, -12.89098713163435228 ) ) ;
#4911 = AXIS2_PLACEMENT_3D ( 'NONE', #3635, #2795, #8428 ) ;
#4912 = DIRECTION ( 'NONE',  ( -1.000000000000000000, 0.000000000000000000, 0.000000000000000000 ) ) ;
#4913 = FACE_OUTER_BOUND ( 'NONE', #8145, .T. ) ;
#4914 = DIRECTION ( 'NONE',  ( -1.000000000000000000, -0.000000000000000000, -0.000000000000000000 ) ) ;
#4915 = DIRECTION ( 'NONE',  ( -1.000000000000000000, -0.000000000000000000, -0.000000000000000000 ) ) ;
#4916 = CARTESIAN_POINT ( 'NONE',  ( -74.37500000204838102, 65.69163855873949842, 25.81189881250000440 ) ) ;
#4917 = CONICAL_SURFACE ( 'NONE', #10820, 5.000000000000000888, 1.047197551196596299 ) ;
#4918 = VERTEX_POINT ( 'NONE', #3161 ) ;
#4919 = CARTESIAN_POINT ( 'NONE',  ( -73.25000000204839523, 65.69163855873948421, -25.81189881250000440 ) ) ;
#4920 = CARTESIAN_POINT ( 'NONE',  ( -76.25000000000000000, 55.00000000000000000, 24.99999999999999645 ) ) ;
#4921 = CARTESIAN_POINT ( 'NONE',  ( 22.23357492888157694, 77.41719160602768568, -11.09194826675321366 ) ) ;
#4922 = CARTESIAN_POINT ( 'NONE',  ( -51.36965469666524342, 68.18978755587353646, 4.719195284573421745 ) ) ;
#4923 = CIRCLE ( 'NONE', #7794, 1.500000000000001332 ) ;
#4924 = LINE ( 'NONE', #11370, #10834 ) ;
#4925 = EDGE_CURVE ( 'NONE', #69, #1770, #5347, .T. ) ;
#4926 = CYLINDRICAL_SURFACE ( 'NONE', #4745, 24.99999999999999645 ) ;
#4927 = ORIENTED_EDGE ( 'NONE', *, *, #643, .F. ) ;
#4928 = CONICAL_SURFACE ( 'NONE', #4355, 3.000000000000000000, 0.9599310885968912466 ) ;
#4929 = CARTESIAN_POINT ( 'NONE',  ( -77.93750000000000000, 72.67766952966368876, 17.67766952966368521 ) ) ;
#4930 = CARTESIAN_POINT ( 'NONE',  ( -73.90625000409680467, 80.00000000000001421, 10.35533905932737397 ) ) ;
#4931 = CIRCLE ( 'NONE', #6273, 1.500000000000001332 ) ;
#4932 = CARTESIAN_POINT ( 'NONE',  ( -50.48899989085627027, 59.74688460148684754, -1.604905836750670778 ) ) ;
#4933 = EDGE_LOOP ( 'NONE', ( #2666, #7561, #5617, #4351 ) ) ;
#4934 = EDGE_CURVE ( 'NONE', #9462, #10179, #10101, .T. ) ;
#4935 = CARTESIAN_POINT ( 'NONE',  ( -6.125254113511556575, 59.17098985002619571, -5.625509189411977751 ) ) ;
#4936 = CARTESIAN_POINT ( 'NONE',  ( 3.000000000000000000, 3.673940397442059868E-16, -5.210428571428570521 ) ) ;
#4937 = VECTOR ( 'NONE', #3666, 1000.000000000000000 ) ;
#4938 = CIRCLE ( 'NONE', #2823, 1.500000000000001332 ) ;
#4939 = ORIENTED_EDGE ( 'NONE', *, *, #5200, .F. ) ;
#4940 = CARTESIAN_POINT ( 'NONE',  ( -2.500000000000000000, 3.061616997868383141E-16, -2.968018054819144158 ) ) ;
#4941 = CARTESIAN_POINT ( 'NONE',  ( -76.34375000204839523, 73.25176868561975141, -18.25176868561974430 ) ) ;
#4942 = ORIENTED_EDGE ( 'NONE', *, *, #1693, .T. ) ;
#4943 = CARTESIAN_POINT ( 'NONE',  ( -63.63584090060282961, 46.00639722032484968, 19.01118640546643590 ) ) ;
#4944 = APPLICATION_CONTEXT ( 'automotive_design' ) ;
#4945 = CARTESIAN_POINT ( 'NONE',  ( -72.40625000204839523, 36.74823131438026280, 18.25176868561974786 ) ) ;
#4946 = CIRCLE ( 'NONE', #1300, 5.000000000000000888 ) ;
#4947 = CARTESIAN_POINT ( 'NONE',  ( -71.09399662003431786, 50.00000004634800632, -0.0006807936302138478625 ) ) ;
#4948 = CARTESIAN_POINT ( 'NONE',  ( -62.51030605291772702, 43.28161195024001273, 17.55542603392786916 ) ) ;
#4949 = CARTESIAN_POINT ( 'NONE',  ( 0.000000000000000000, 0.000000000000000000, 0.000000000000000000 ) ) ;
#4950 = ORIENTED_EDGE ( 'NONE', *, *, #439, .F. ) ;
#4951 = CARTESIAN_POINT ( 'NONE',  ( 0.000000000000000000, -24.99999999999999645, 0.000000000000000000 ) ) ;
#4952 = FACE_OUTER_BOUND ( 'NONE', #2652, .T. ) ;
#4953 = CARTESIAN_POINT ( 'NONE',  ( -15.14429485721040614, 76.01882847486140804, 2.745652427074330326 ) ) ;
#4954 = ORIENTED_EDGE ( 'NONE', *, *, #8773, .T. ) ;
#4955 = CARTESIAN_POINT ( 'NONE',  ( -4.941614180435440318, 57.05942949522437146, -21.01535240110448299 ) ) ;
#4956 = CARTESIAN_POINT ( 'NONE',  ( -27.12710454428388118, 47.94392800691067436, 12.25026322333570228 ) ) ;
#4957 = FACE_OUTER_BOUND ( 'NONE', #7189, .T. ) ;
#4958 = FACE_OUTER_BOUND ( 'NONE', #348, .T. ) ;
#4959 = UNCERTAINTY_MEASURE_WITH_UNIT (LENGTH_MEASURE( 1.000000000000000082E-05 ), #4474, 'distance_accuracy_value', 'NONE');
#4960 = PLANE ( 'NONE',  #1335 ) ;
#4961 = AXIS2_PLACEMENT_3D ( 'NONE', #2614, #1710, #6397 ) ;
#4962 = VERTEX_POINT ( 'NONE', #6283 ) ;
#4963 = CARTESIAN_POINT ( 'NONE',  ( -78.68750000000001421, 37.32233047033631124, -17.67766952966368166 ) ) ;
#4964 = CARTESIAN_POINT ( 'NONE',  ( -62.57658715170816066, 54.99925176542368632, 0.005738867717030676080 ) ) ;
#4965 = FACE_OUTER_BOUND ( 'NONE', #3678, .T. ) ;
#4966 = CIRCLE ( 'NONE', #8299, 4.999999999999997335 ) ;
#4967 = CIRCLE ( 'NONE', #11640, 2.500000000000000000 ) ;
#4968 = LINE ( 'NONE', #2322, #10843 ) ;
#4969 = CARTESIAN_POINT ( 'NONE',  ( -16.55667896787908333, 61.80197853705212907, 1.825560432032844460 ) ) ;
#4970 = AXIS2_PLACEMENT_3D ( 'NONE', #8670, #2310, #4061 ) ;
#4971 = ORIENTED_EDGE ( 'NONE', *, *, #11272, .T. ) ;
#4972 = CARTESIAN_POINT ( 'NONE',  ( -19.63602748969081446, 62.08618401115764129, 19.80343740535094099 ) ) ;
#4973 = DIRECTION ( 'NONE',  ( -0.000000000000000000, -0.000000000000000000, -1.000000000000000000 ) ) ;
#4974 = CARTESIAN_POINT ( 'NONE',  ( -2.500000000000005773, -4.330127018922191873, 0.000000000000000000 ) ) ;
#4975 = CARTESIAN_POINT ( 'NONE',  ( -78.68750000204839523, 65.69163855873949842, 25.81189881250000084 ) ) ;
#4976 = CARTESIAN_POINT ( 'NONE',  ( -24.25189443604024575, 79.11314215675321293, 6.649975675490534144 ) ) ;
#4977 = CARTESIAN_POINT ( 'NONE',  ( -79.25000000204838102, 65.69163855873948421, -25.81189881250000440 ) ) ;
#4978 = VERTEX_POINT ( 'NONE', #9914 ) ;
#4979 = EDGE_CURVE ( 'NONE', #8998, #6548, #7073, .T. ) ;
#4980 = CARTESIAN_POINT ( 'NONE',  ( -72.21875000204838102, 29.18810118750000271, 4.741568889096522788E-15 ) ) ;
#4981 = AXIS2_PLACEMENT_3D ( 'NONE', #11228, #4841, #10510 ) ;
#4982 = DIRECTION ( 'NONE',  ( -1.000000000000000000, -6.033820786006286457E-17, -0.000000000000000000 ) ) ;
#4983 = CONICAL_SURFACE ( 'NONE', #11653, 3.000000000000000000, 0.9599310885968912466 ) ;
#4984 = CARTESIAN_POINT ( 'NONE',  ( -5.337209886265139147, 63.04750289227570192, -19.42727033598380970 ) ) ;
#4985 = FACE_OUTER_BOUND ( 'NONE', #8973, .T. ) ;
#4986 = DIRECTION ( 'NONE',  ( -1.000000000000000000, -0.000000000000000000, -0.000000000000000000 ) ) ;
#4987 = DIRECTION ( 'NONE',  ( 1.000000000000000000, 6.033820786006286457E-17, -0.000000000000000000 ) ) ;
#4988 = AXIS2_PLACEMENT_3D ( 'NONE', #8978, #10936, #7188 ) ;
#4989 = ORIENTED_EDGE ( 'NONE', *, *, #4330, .F. ) ;
#4990 = CARTESIAN_POINT ( 'NONE',  ( -77.00000000000000000, 55.00000000000000000, -24.99999999999999645 ) ) ;
#4991 = DIRECTION ( 'NONE',  ( 1.000000000000000000, 0.000000000000000000, 0.000000000000000000 ) ) ;
#4992 = CARTESIAN_POINT ( 'NONE',  ( 25.00000000000000000, 76.00000000000000000, 0.000000000000000000 ) ) ;
#4993 = ORIENTED_EDGE ( 'NONE', *, *, #11634, .F. ) ;
#4994 = EDGE_CURVE ( 'NONE', #7792, #306, #6452, .T. ) ;
#4995 = CARTESIAN_POINT ( 'NONE',  ( 6.417054786244230868, 48.01588556897357307, -0.6870108247934131329 ) ) ;
#4996 = VECTOR ( 'NONE', #1151, 1000.000000000000000 ) ;
#4997 = FACE_OUTER_BOUND ( 'NONE', #5206, .T. ) ;
#4998 = DIRECTION ( 'NONE',  ( -1.000000000000000000, -0.000000000000000000, -0.000000000000000000 ) ) ;
#4999 = B_SPLINE_SURFACE_WITH_KNOTS ( 'NONE', 3, 3, ( 
 ( #8681, #11413, #3223, #2328, #637, #7008, #5998, #9632, #1427, #4244, #4182, #7843, #4300, #2445, #11472, #3283, #6953, #10578, #2379, #2682, #7303, #9086, #9200, #5322, #9143, #5494, #4592, #6229, #2794, #8975, #751, #4651, #4479, #10869, #925, #810, #3634, #864, #8131, #4426, #11656, #8249, #990, #3466, #25, #4536, #11769, #6288, #7131, #6460, #10088, #10932, #2562, #8083, #3693, #11827, #3577, #6348, #10982, #7247, #1886, #5556, #8191, #11716, #9977, #9860, #9919, #1717, #1825, #7357, #10031, #10753, #2742, #6401, #1654, #3516, #1772, #7185, #10810, #2620, #5383, #9033, #5438, #11044, #1290, #3748, #10334, #9319, #8304, #5804, #2852, #7482, #11104, #1048, #5741, #7416, #8427, #8546, #10272, #11286, #6521, #9258, #10151, #2132, #3100, #1950, #4771, #5619, #6765, #6640, #212, #329, #7653, #3876, #2918, #6583, #8490, #4713, #9377, #8365, #2070, #85, #7537, #146 ),
 ( #3814, #10213, #1171, #4838, #5860, #3993, #6704, #268, #2006, #11159, #9438, #5678, #1227, #10392, #1107, #7595, #4894, #2974, #3931, #11225, #2188, #9499, #3034, #8613, #9729, #6995, #9676, #2248, #10446, #390, #11459, #1355, #11580, #2429, #3268, #7890, #7827, #11521, #3327, #5917, #6939, #564, #2368, #2492, #9562, #6097, #10618, #1529, #11344, #7946, #5022, #8669, #9792, #9620, #4166, #5193, #5986, #8783, #6040, #1415, #450, #4956, #8845, #6157, #4059, #624, #1472, #5078, #11396, #7715, #3382, #7059, #4231, #3152, #4107, #4288, #5135, #8721, #10567, #10679, #504, #6820, #7765, #3210, #6878, #10506, #2309, #680, #4353, #7117, #10742, #2549, #6215, #11639, #3445, #1585, #5253, #8900, #8004, #9267, #11117, #1186, #1059, #10287, #10166, #11172, #4661, #4786, #1962, #3887, #11058, #11235, #5630, #10348, #3046, #2145, #9452, #9392, #10403, #7549, #6596, #1119, #280, #2203 ),
 ( #4725, #2987, #1002, #6716, #2080, #6775, #3829, #5815, #5870, #3110, #3943, #7494, #5692, #4908, #6653, #2929, #10225, #2867, #8500, #5755, #340, #4851, #7606, #8378, #1238, #224, #6534, #8443, #8314, #2018, #8559, #95, #158, #7665, #4005, #11300, #3763, #7431, #9330, #3394, #10457, #634, #10627, #8855, #3163, #5143, #4969, #2376, #11410, #8621, #1483, #9572, #8733, #7778, #2504, #461, #6888, #4241, #5995, #574, #3335, #9686, #9511, #3220, #4296, #7955, #8795, #1302, #403, #11589, #10516, #7068, #4068, #7725, #7900, #10692, #11355, #6833, #5205, #6107, #2259, #4179, #6949, #1369, #8678, #5930, #5032, #4117, #11529, #2323, #9629, #1424, #5087, #516, #7839, #11468, #1538, #3279, #10575, #6051, #7005, #2441, #9740, #5378, #4422, #10979, #8972, #3513, #860, #2616, #9082, #11824, #6343, #6169, #8079, #9139, #921, #1769, #9800, #1594, #4589, #11713, #8245, #690 ),
 ( #5490, #3573, #7243, #22, #3690, #8128, #4532, #2559, #7354, #4362, #747, #10806, #8909, #5262, #8014, #8187, #7182, #11652, #3630, #3461, #5319, #6285, #10750, #10866, #7128, #9916, #6398, #11765, #6226, #1713, #4476, #2678, #9030, #9857, #9974, #1650, #806, #5434, #7299, #10929, #2739, #1820, #10028, #872, #220, #8434, #1056, #6528, #5626, #5686, #3642, #1894, #10877, #4720, #8310, #4780, #1833, #8374, #3883, #1116, #10160, #5503, #3700, #2925, #9209, #9150, #934, #4544, #1957, #4657, #10221, #7426, #9263, #2749, #154, #10096, #9092, #10989, #2688, #4599, #7489, #6354, #6407, #9326, #91, #998, #9983, #2013, #8256, #1778, #11833, #5445, #3820, #8199, #7310, #11111, #10939, #3757, #32, #5563, #10039, #7364, #6591, #11052, #2803, #2860, #6467, #2254, #4846, #10398, #3158, #4964, #5084, #1179, #5029, #1362, #457, #2076, #10513, #8497, #276, #511, #336, #6773 ) ),
 .UNSPECIFIED., .F., .F., .F.,
 ( 4, 4 ),
 ( 4, 2, 2, 2, 2, 2, 2, 2, 2, 2, 2, 2, 2, 2, 2, 2, 2, 2, 2, 2, 2, 2, 2, 2, 2, 2, 2, 2, 2, 2, 2, 2, 2, 2, 2, 2, 2, 2, 2, 2, 2, 2, 2, 2, 2, 2, 2, 2, 2, 2, 2, 2, 2, 2, 2, 2, 2, 2, 2, 2, 2, 4 ),
 ( 0.000000000000000000, 1.000000000000000000 ),
 ( 0.000000000000000000, 0.02499977550252127645, 0.04999988577693819519, 0.07499999605135511394, 0.09999999831535408279, 0.1250000005793530378, 0.1500000028441162425, 0.1750000051088794195, 0.1937500039558066045, 0.2031250033792701970, 0.2125000028027338173, 0.2218750022261974375, 0.2312500016496610300, 0.2500000004965882150, 0.2750000027613288545, 0.3000000050260694384, 0.3187500038730080032, 0.3281250032964772578, 0.3375000027199465125, 0.3468750021434158226, 0.3562500015668850772, 0.3750000004138236420, 0.4000000026785641705, 0.4250000049433046989, 0.4437500037902432082, 0.4531250032137125183, 0.4625000026371817730, 0.4718750020606510276, 0.4812500014841203377, 0.5000000003310588470, 0.5250000025957997085, 0.5500000048605405700, 0.5687500037074788573, 0.5781250031309480564, 0.5875000025544172555, 0.5968750019778864546, 0.6062500014013556537, 0.6250000002482940520, 0.6500000025128280789, 0.6750000047773621059, 0.6937500036244039769, 0.7031250030479249125, 0.7125000024714458480, 0.7218750018949667835, 0.7312500013184877190, 0.7500000001655295900, 0.7750000023794885173, 0.8000000045934475557, 0.8187500034657768655, 0.8281250029019414649, 0.8375000023381060643, 0.8468750017742707747, 0.8562500012104353742, 0.8750000000827646840, 0.8937502654913498379, 0.9031253981956424148, 0.9125005308999349918, 0.9218756636042275687, 0.9312507963085201457, 0.9500010617171052996, 0.9750005308585526498, 1.000000000000000000 ),
 .UNSPECIFIED. ) ;
#5000 = ORIENTED_EDGE ( 'NONE', *, *, #7637, .T. ) ;
#5001 = CARTESIAN_POINT ( 'NONE',  ( 18.41311296310942325, 74.28344047684244345, -10.65941174978863337 ) ) ;
#5002 = AXIS2_PLACEMENT_3D ( 'NONE', #4717, #1576, #2414 ) ;
#5003 = CARTESIAN_POINT ( 'NONE',  ( -75.59375000204839523, 36.74823131438026280, 18.25176868561974786 ) ) ;
#5004 = ADVANCED_FACE ( 'NONE', ( #4588 ), #7638, .T. ) ;
#5005 = VERTEX_POINT ( 'NONE', #9855 ) ;
#5006 = CARTESIAN_POINT ( 'NONE',  ( -58.05785365788000263, 64.93276152744238061, 18.60033633024681521 ) ) ;
#5007 = CONICAL_SURFACE ( 'NONE', #8638, 2.500000000000000000, 0.9599310885968755924 ) ;
#5008 = CARTESIAN_POINT ( 'NONE',  ( -72.59375000204838102, 55.00000000000000000, 25.81189881249999729 ) ) ;
#5009 = CARTESIAN_POINT ( 'NONE',  ( -78.00000000000002842, 46.51471862576140381, -1.499996628082201244 ) ) ;
#5010 = DIRECTION ( 'NONE',  ( 0.000000000000000000, 1.000000000000000000, 0.000000000000000000 ) ) ;
#5011 = AXIS2_PLACEMENT_3D ( 'NONE', #3358, #714, #7980 ) ;
#5012 = CONICAL_SURFACE ( 'NONE', #11686, 2.500000000000000000, 0.9599310885968755924 ) ;
#5013 =( LENGTH_UNIT ( ) NAMED_UNIT ( * ) SI_UNIT ( .MILLI., .METRE. ) );
#5014 = DIRECTION ( 'NONE',  ( -1.000000000000000000, 0.000000000000000000, 0.000000000000000000 ) ) ;
#5015 = ADVANCED_FACE ( 'NONE', ( #3459 ), #5488, .F. ) ;
#5016 = ORIENTED_EDGE ( 'NONE', *, *, #9614, .T. ) ;
#5017 = DIRECTION ( 'NONE',  ( -1.000000000000000000, -0.000000000000000000, -0.000000000000000000 ) ) ;
#5018 = CARTESIAN_POINT ( 'NONE',  ( -31.26269038945179446, 34.87416470039633509, 6.107602927758665423 ) ) ;
#5019 = ORIENTED_EDGE ( 'NONE', *, *, #7133, .T. ) ;
#5020 = AXIS2_PLACEMENT_3D ( 'NONE', #9927, #11725, #646 ) ;
#5021 = CARTESIAN_POINT ( 'NONE',  ( 2.670522128595300249, 35.57712497142318142, -8.044658458458092909 ) ) ;
#5022 = CARTESIAN_POINT ( 'NONE',  ( -19.33520177743824320, 64.91269256302088309, 9.913189658205579846 ) ) ;
#5023 = AXIS2_PLACEMENT_3D ( 'NONE', #3414, #7027, #5279 ) ;
#5024 = CARTESIAN_POINT ( 'NONE',  ( 3.000000000000000000, 3.673940397442059868E-16, -1.753742857142857048 ) ) ;
#5025 = CARTESIAN_POINT ( 'NONE',  ( -75.12500000409677625, 55.00000000000000000, 24.99999999999999645 ) ) ;
#5026 = CARTESIAN_POINT ( 'NONE',  ( 46.99999999999999289, 58.53553390593273065, 3.535533905932731091 ) ) ;
#5027 = ORIENTED_EDGE ( 'NONE', *, *, #9234, .F. ) ;
#5028 = CARTESIAN_POINT ( 'NONE',  ( -73.71875000000000000, 80.00000000000001421, -10.35533905932737753 ) ) ;
#5029 = CARTESIAN_POINT ( 'NONE',  ( -63.75812180237208793, 55.00413150893107428, -0.006526425526955113854 ) ) ;
#5030 = CYLINDRICAL_SURFACE ( 'NONE', #2663, 4.999999999999997335 ) ;
#5031 = FACE_OUTER_BOUND ( 'NONE', #7082, .T. ) ;
#5032 = CARTESIAN_POINT ( 'NONE',  ( -44.75046787418907712, 57.03233382151384490, -6.700212328598206035 ) ) ;
#5033 = ORIENTED_EDGE ( 'NONE', *, *, #5587, .F. ) ;
#5034 = CARTESIAN_POINT ( 'NONE',  ( -16.69731055678936826, 70.57278980777935828, 14.11442052818484783 ) ) ;
#5035 = DIRECTION ( 'NONE',  ( -1.000000000000000000, 0.000000000000000000, 0.000000000000000000 ) ) ;
#5036 = CARTESIAN_POINT ( 'NONE',  ( 52.99999999999999289, 58.53553390593273065, 3.535533905932731091 ) ) ;
#5037 = CARTESIAN_POINT ( 'NONE',  ( -78.21875000204839523, 29.18810118750000271, 4.741568889096522788E-15 ) ) ;
#5038 = CARTESIAN_POINT ( 'NONE',  ( -21.38022012555706652, 76.71392452634511017, 12.39514039398179968 ) ) ;
#5039 = CARTESIAN_POINT ( 'NONE',  ( -75.59375000204839523, 55.00000000000000000, 25.81189881249999729 ) ) ;
#5040 = ORIENTED_EDGE ( 'NONE', *, *, #10185, .T. ) ;
#5041 = CARTESIAN_POINT ( 'NONE',  ( -76.71875000409679046, 65.35533905932737753, 24.99999999999999645 ) ) ;
#5042 = FACE_BOUND ( 'NONE', #11269, .T. ) ;
#5043 = FACE_BOUND ( 'NONE', #10167, .T. ) ;
#5044 = SURFACE_STYLE_USAGE ( .BOTH. , #9525 ) ;
#5045 = CARTESIAN_POINT ( 'NONE',  ( -27.49360061100878738, 37.45598436699922473, 11.71495266747331421 ) ) ;
#5046 = DIRECTION ( 'NONE',  ( 0.000000000000000000, 1.000000000000000000, 0.000000000000000000 ) ) ;
#5047 = PLANE ( 'NONE',  #5690 ) ;
#5048 = CARTESIAN_POINT ( 'NONE',  ( -73.90625000000007105, 65.35533905932732068, -24.99999999999986500 ) ) ;
#5049 = ORIENTED_EDGE ( 'NONE', *, *, #6777, .F. ) ;
#5050 = CARTESIAN_POINT ( 'NONE',  ( -78.00000000000001421, 67.72792206135787296, 4.242644059037073312 ) ) ;
#5051 = CARTESIAN_POINT ( 'NONE',  ( -76.25000000000000000, 55.00000000000000000, 24.99999999999999645 ) ) ;
#5052 = FACE_OUTER_BOUND ( 'NONE', #10072, .T. ) ;
#5053 = CARTESIAN_POINT ( 'NONE',  ( -44.65600760483433618, 56.29883701348843772, -4.839347163649881267 ) ) ;
#5054 = ORIENTED_EDGE ( 'NONE', *, *, #3285, .F. ) ;
#5055 = EDGE_CURVE ( 'NONE', #2528, #9349, #8785, .T. ) ;
#5056 = CARTESIAN_POINT ( 'NONE',  ( -60.66697644449794780, 52.31984451244050405, 6.470678962653597210 ) ) ;
#5057 = CARTESIAN_POINT ( 'NONE',  ( -71.18677368791114191, 77.11938847399009944, 12.77062708069394503 ) ) ;
#5058 = DIRECTION ( 'NONE',  ( -1.000000000000000000, -0.000000000000000000, -0.000000000000000000 ) ) ;
#5059 = ORIENTED_EDGE ( 'NONE', *, *, #4379, .T. ) ;
#5060 = CARTESIAN_POINT ( 'NONE',  ( -4.067038661182964928E-21, 64.99605696851786263, 19.59792961213366169 ) ) ;
#5061 = CARTESIAN_POINT ( 'NONE',  ( 0.000000000000000000, 0.000000000000000000, -3.996153373752295401 ) ) ;
#5062 = ORIENTED_EDGE ( 'NONE', *, *, #10409, .T. ) ;
#5063 = VECTOR ( 'NONE', #8132, 1000.000000000000000 ) ;
#5064 = CARTESIAN_POINT ( 'NONE',  ( -72.96875000204838102, 80.81189881250000440, -1.580522963032174394E-15 ) ) ;
#5065 = EDGE_CURVE ( 'NONE', #6710, #494, #9080, .T. ) ;
#5066 = EDGE_CURVE ( 'NONE', #9906, #4880, #5733, .T. ) ;
#5067 = EDGE_CURVE ( 'NONE', #2603, #9484, #11764, .T. ) ;
#5068 = DIRECTION ( 'NONE',  ( -1.000000000000000000, -0.000000000000000000, -0.000000000000000000 ) ) ;
#5069 = CARTESIAN_POINT ( 'NONE',  ( -4.331185467099802899, 55.00135650712124402, -0.002828848648976476851 ) ) ;
#5070 = DIRECTION ( 'NONE',  ( -1.000000000000000000, -0.000000000000000000, -0.000000000000000000 ) ) ;
#5071 = VERTEX_POINT ( 'NONE', #11711 ) ;
#5072 = CARTESIAN_POINT ( 'NONE',  ( -4.592054218142292754, -3.122278952918454920, -0.3106000600989325400 ) ) ;
#5073 = EDGE_CURVE ( 'NONE', #52, #6548, #5433, .T. ) ;
#5074 = CARTESIAN_POINT ( 'NONE',  ( -44.96936008568403764, 63.99178041037959019, -19.01235157881157178 ) ) ;
#5075 = EDGE_CURVE ( 'NONE', #3587, #10599, #10927, .T. ) ;
#5076 = ORIENTED_EDGE ( 'NONE', *, *, #10514, .F. ) ;
#5077 = CARTESIAN_POINT ( 'NONE',  ( 15.14427135698260507, 57.74566953878471054, 20.97954867241053023 ) ) ;
#5078 = CARTESIAN_POINT ( 'NONE',  ( -31.58948382711383118, 41.58084601413256820, 4.072244092560330486 ) ) ;
#5079 = CARTESIAN_POINT ( 'NONE',  ( 0.000000000000000000, -30.00000000000000000, -5.000000000000000000 ) ) ;
#5080 = ADVANCED_FACE ( 'NONE', ( #5260 ), #1768, .F. ) ;
#5081 = CARTESIAN_POINT ( 'NONE',  ( -25.98930196984718322, 53.70295539467162627, 4.839812903858289772 ) ) ;
#5082 = ORIENTED_EDGE ( 'NONE', *, *, #9241, .T. ) ;
#5083 = CARTESIAN_POINT ( 'NONE',  ( -74.65625000000000000, 44.64466094067262958, 25.00000000000001066 ) ) ;
#5084 = CARTESIAN_POINT ( 'NONE',  ( -62.87201990682712704, 55.00012644727732436, 0.002206787302671962998 ) ) ;
#5085 = VECTOR ( 'NONE', #8305, 1000.000000000000000 ) ;
#5086 = LINE ( 'NONE', #10574, #7800 ) ;
#5087 = CARTESIAN_POINT ( 'NONE',  ( -49.22341880855515939, 61.10062350524368924, -3.518778999107284200 ) ) ;
#5088 = ORIENTED_EDGE ( 'NONE', *, *, #55, .F. ) ;
#5089 = CARTESIAN_POINT ( 'NONE',  ( -48.85567157503042779, 75.97628680226326026, -2.745941867523475466 ) ) ;
#5090 = CARTESIAN_POINT ( 'NONE',  ( -75.00000000000001421, 42.56479188213557308, 21.68791366326873060 ) ) ;
#5091 = DIRECTION ( 'NONE',  ( -1.000000000000000000, 0.000000000000000000, 0.000000000000000000 ) ) ;
#5092 = CARTESIAN_POINT ( 'NONE',  ( -75.96875000204839523, 80.81189881250000440, -1.580522963032174394E-15 ) ) ;
#5093 =( BOUNDED_CURVE ( )  B_SPLINE_CURVE ( 2, ( #10431, #11443, #9545, #3979, #3194, #6866, #4213, #433, #1213, #9659, #7696, #4879, #8529, #11506, #6803, #3314, #7636, #11268, #493, #6981, #3079, #7876, #10490, #5972, #6750, #10378, #9608, #6925, #9483, #2173, #5842, #11329, #5902, #1272, #4941, #8598, #2355, #2233, #373, #6024, #3137, #1341, #5003, #8653, #1457, #5120, #7158, #7043, #8046, #1512, #1625, #10665, #722, #7932, #8108, #2474, #7218, #11744, #10844, #6317, #6261, #5570, #3547, #2594, #6140, #9836, #2651, #9716, #9949, #1005, #5176, #9004, #1902, #8946, #8831, #11687, #9217, #4665, #11061, #612, #8317, #665, #2535, #98, #3493, #4335, #7986 ),
 .UNSPECIFIED., .F., .T. ) 
 B_SPLINE_CURVE_WITH_KNOTS ( ( 3, 2, 2, 2, 2, 2, 2, 2, 2, 2, 2, 2, 2, 2, 2, 2, 2, 2, 2, 2, 2, 2, 2, 2, 2, 2, 2, 2, 2, 2, 2, 2, 2, 2, 2, 2, 2, 2, 2, 2, 2, 2, 2, 3 ),
 ( 0.000000000000000000, 0.02083333333333333218, 0.04166666666666666435, 0.06250000000000000000, 0.08333333333333332871, 0.1041666666666666713, 0.1250000000000000000, 0.1458333333333333426, 0.1666666666666666574, 0.1875000000000000000, 0.2083333333333333426, 0.2291666666666666297, 0.2500000000000000000, 0.2708333333333333148, 0.2916666666666666852, 0.3125000000000000000, 0.3333333333333333148, 0.3541666666666666852, 0.3750000000000000000, 0.3958333333333333148, 0.4166666666666666852, 0.4375000000000000000, 0.4583333333333332593, 0.4791666666666666852, 0.5000000000000000000, 0.5208333333333333703, 0.5416666666666666297, 0.5625000000000000000, 0.5833333333333333703, 0.6041666666666666297, 0.6250000000000000000, 0.6458333333333333703, 0.6666666666666666297, 0.6875000000000000000, 0.7083333333333333703, 0.7291666666666666297, 0.7500000000000000000, 0.7708333333333333703, 0.7916666666666666297, 0.8125000000000000000, 0.8333333333333333703, 0.8541666666666667407, 0.8750000000000000000, 0.8888490471511721891 ),
 .UNSPECIFIED. ) 
 CURVE ( )  GEOMETRIC_REPRESENTATION_ITEM ( )  RATIONAL_B_SPLINE_CURVE ( ( 1.000000000000000000, 0.9238795325112867385, 1.000000000000000000, 0.9238795325112867385, 1.000000000000000000, 0.9238795325112867385, 1.000000000000000000, 0.9238795325112867385, 1.000000000000000000, 0.9238795325112867385, 1.000000000000000000, 0.9238795325112867385, 1.000000000000000000, 0.9238795325112867385, 1.000000000000000000, 0.9238795325112867385, 1.000000000000000000, 0.9238795325112867385, 1.000000000000000000, 0.9238795325112867385, 1.000000000000000000, 0.9238795325112867385, 1.000000000000000000, 0.9238795325112867385, 1.000000000000000000, 0.9238795325112867385, 1.000000000000000000, 0.9238795325112867385, 1.000000000000000000, 0.9238795325112867385, 1.000000000000000000, 0.9238795325112867385, 1.000000000000000000, 0.9238795325112867385, 1.000000000000000000, 0.9238795325112867385, 1.000000000000000000, 0.9238795325112867385, 1.000000000000000000, 0.9238795325112867385, 1.000000000000000000, 0.9238795325112867385, 1.000000000000000000, 0.9238795325112867385, 1.000000000000000000, 0.9238795325112867385, 1.000000000000000000, 0.9238795325112867385, 1.000000000000000000, 0.9238795325112867385, 1.000000000000000000, 0.9238795325112867385, 1.000000000000000000, 0.9238795325112867385, 1.000000000000000000, 0.9238795325112867385, 1.000000000000000000, 0.9238795325112867385, 1.000000000000000000, 0.9238795325112867385, 1.000000000000000000, 0.9238795325112867385, 1.000000000000000000, 0.9238795325112867385, 1.000000000000000000, 0.9238795325112867385, 1.000000000000000000, 0.9238795325112867385, 1.000000000000000000, 0.9238795325112867385, 1.000000000000000000, 0.9238795325112867385, 1.000000000000000000, 0.9238795325112867385, 1.000000000000000000, 0.9238795325112867385, 1.000000000000000000, 0.9238795325112867385, 1.000000000000000000, 0.9238795325112867385, 1.000000000000000000, 0.9238795325112867385, 1.000000000000000000, 0.9238795325112867385, 1.000000000000000000, 0.9493985947158180005, 0.9660721892104719988 ) ) 
 REPRESENTATION_ITEM ( '' )  );
#5094 = CARTESIAN_POINT ( 'NONE',  ( -21.60181664749086039, 76.89598700960922883, 12.07086080051332644 ) ) ;
#5095 = CARTESIAN_POINT ( 'NONE',  ( -74.65625000204839523, 73.25176868561975141, -18.25176868561974430 ) ) ;
#5096 = PRODUCT_DEFINITION_FORMATION_WITH_SPECIFIED_SOURCE ( 'ANY', '', #10824, .NOT_KNOWN. ) ;
#5097 = EDGE_LOOP ( 'NONE', ( #10727, #2495, #974, #11366 ) ) ;
#5098 = CARTESIAN_POINT ( 'NONE',  ( -73.43750000409677625, 37.32233047033631124, 17.67766952966369232 ) ) ;
#5099 = CARTESIAN_POINT ( 'NONE',  ( 0.000000000000000000, 0.000000000000000000, -3.482085714285714229 ) ) ;
#5100 = EDGE_LOOP ( 'NONE', ( #2877, #1287, #6475, #7057 ) ) ;
#5101 = AXIS2_PLACEMENT_3D ( 'NONE', #1372, #7783, #5035 ) ;
#5102 = CARTESIAN_POINT ( 'NONE',  ( -22.47759590436300314, 52.25445647903773505, 21.02373912143526979 ) ) ;
#5103 = CARTESIAN_POINT ( 'NONE',  ( -75.50000000000001421, 54.99999999999944578, -24.99999999999999645 ) ) ;
#5104 = CARTESIAN_POINT ( 'NONE',  ( -75.49999999999972999, 55.00000000002793854, -24.99999999999999645 ) ) ;
#5105 = CARTESIAN_POINT ( 'NONE',  ( -73.81250000000008527, 72.67766952966360350, -17.67766952966359639 ) ) ;
#5106 = ORIENTED_EDGE ( 'NONE', *, *, #6601, .T. ) ;
#5107 = AXIS2_PLACEMENT_3D ( 'NONE', #498, #4159, #5014 ) ;
#5108 = DIRECTION ( 'NONE',  ( -1.000000000000000000, -0.000000000000000000, -0.000000000000000000 ) ) ;
#5109 = CARTESIAN_POINT ( 'NONE',  ( -74.46875000000000000, 30.00000000000001421, 10.35533905932739174 ) ) ;
#5110 = FACE_OUTER_BOUND ( 'NONE', #10226, .T. ) ;
#5111 = CARTESIAN_POINT ( 'NONE',  ( 0.000000000000000000, 0.000000000000000000, -0.8895714285714284575 ) ) ;
#5112 = EDGE_LOOP ( 'NONE', ( #2231, #7849, #675, #9188 ) ) ;
#5113 = EDGE_CURVE ( 'NONE', #2768, #9484, #3511, .T. ) ;
#5114 = CARTESIAN_POINT ( 'NONE',  ( -52.79191841873938529, 60.62555712573470856, 4.171026843566116860 ) ) ;
#5115 = LINE ( 'NONE', #1621, #4809 ) ;
#5116 =( NAMED_UNIT ( * ) PLANE_ANGLE_UNIT ( ) SI_UNIT ( $, .RADIAN. ) );
#5117 = VERTEX_POINT ( 'NONE', #11823 ) ;
#5118 = CARTESIAN_POINT ( 'NONE',  ( 5.688665219163724807, 66.14467445454752692, -18.96884555856732035 ) ) ;
#5119 = AXIS2_PLACEMENT_3D ( 'NONE', #2457, #1609, #5276 ) ;
#5120 = CARTESIAN_POINT ( 'NONE',  ( -75.31250000204839523, 29.18810118750000626, -10.69163855873949132 ) ) ;
#5121 = CIRCLE ( 'NONE', #127, 5.000000000000000888 ) ;
#5122 = VERTEX_POINT ( 'NONE', #9138 ) ;
#5123 = CARTESIAN_POINT ( 'NONE',  ( -73.81250000204839523, 29.18810118750000981, 10.69163855873950020 ) ) ;
#5124 = CARTESIAN_POINT ( 'NONE',  ( 9.999999999999994671, 0.000000000000000000, 10.00000000000000000 ) ) ;
#5125 = CARTESIAN_POINT ( 'NONE',  ( -75.50000000409677625, 80.00000000000000000, -1.530808498934191324E-15 ) ) ;
#5126 = CARTESIAN_POINT ( 'NONE',  ( -17.46186840051235123, 54.99807057725060133, -0.005246742405310452287 ) ) ;
#5127 = CARTESIAN_POINT ( 'NONE',  ( 0.000000000000000000, 0.000000000000000000, 0.000000000000000000 ) ) ;
#5128 = STYLED_ITEM ( 'NONE', ( #7177 ), #9980 ) ;
#5129 = CARTESIAN_POINT ( 'NONE',  ( -75.00000000000000000, 31.58343112012256526, 9.522673556080674118 ) ) ;
#5130 = ORIENTED_EDGE ( 'NONE', *, *, #3370, .T. ) ;
#5131 = CARTESIAN_POINT ( 'NONE',  ( -78.00000000000001421, 59.24264068711928388, -12.72791868944003824 ) ) ;
#5132 = CARTESIAN_POINT ( 'NONE',  ( -21.32947787934852357, 63.04568470447853912, 19.42265540296757464 ) ) ;
#5133 = ORIENTED_EDGE ( 'NONE', *, *, #7055, .T. ) ;
#5134 = CARTESIAN_POINT ( 'NONE',  ( -9.302693722564239209, 70.58343099003624843, -14.12448736900078572 ) ) ;
#5135 = CARTESIAN_POINT ( 'NONE',  ( -37.20624055104932637, 43.81852209390767428, -8.592061044857116414 ) ) ;
#5136 = CARTESIAN_POINT ( 'NONE',  ( -74.37500000204838102, 65.69163855873949842, 25.81189881250000440 ) ) ;
#5137 = ORIENTED_EDGE ( 'NONE', *, *, #6473, .T. ) ;
#5138 = CARTESIAN_POINT ( 'NONE',  ( -77.28125000204838102, 55.00000000000000000, 25.81189881249999729 ) ) ;
#5139 = DIRECTION ( 'NONE',  ( 0.000000000000000000, 0.000000000000000000, 1.000000000000000000 ) ) ;
#5140 = ADVANCED_FACE ( 'NONE', ( #920 ), #8127, .F. ) ;
#5141 = SURFACE_STYLE_FILL_AREA ( #7775 ) ;
#5142 = CARTESIAN_POINT ( 'NONE',  ( 12.14951178748830785, 51.69754629963415482, 3.768454028063179972 ) ) ;
#5143 = CARTESIAN_POINT ( 'NONE',  ( -15.77658089785693996, 62.01719014345248837, 0.9163230061594601628 ) ) ;
#5144 = ORIENTED_EDGE ( 'NONE', *, *, #7570, .F. ) ;
#5145 = CARTESIAN_POINT ( 'NONE',  ( -15.27494751580540111, 73.62981360231496808, 9.945832149094092856 ) ) ;
#5146 = DIRECTION ( 'NONE',  ( 0.000000000000000000, 1.000000000000000000, 0.000000000000000000 ) ) ;
#5147 = CARTESIAN_POINT ( 'NONE',  ( -70.34104699118842063, 33.99562393659818582, 0.006612473344882202446 ) ) ;
#5148 = EDGE_CURVE ( 'NONE', #8424, #306, #3998, .T. ) ;
#5149 = CARTESIAN_POINT ( 'NONE',  ( -78.78125000204839523, 73.25176868561975141, 18.25176868561974075 ) ) ;
#5150 = FACE_OUTER_BOUND ( 'NONE', #6292, .T. ) ;
#5151 = CARTESIAN_POINT ( 'NONE',  ( -73.25000000204839523, 65.69163855873948421, -25.81189881250000440 ) ) ;
#5152 = ORIENTED_EDGE ( 'NONE', *, *, #7542, .F. ) ;
#5153 = CARTESIAN_POINT ( 'NONE',  ( -75.40625000409677625, 80.00000000000001421, 10.35533905932737397 ) ) ;
#5154 = CARTESIAN_POINT ( 'NONE',  ( -15.00000000000000355, 5.000000000000000000, -29.99999999999999289 ) ) ;
#5155 = CARTESIAN_POINT ( 'NONE',  ( -5.000000000000000000, -2.886751345948133540, -6.099999999999999645 ) ) ;
#5156 = CARTESIAN_POINT ( 'NONE',  ( -17.00387655282055377, 69.86881140706658755, 14.86941770366936311 ) ) ;
#5157 = CARTESIAN_POINT ( 'NONE',  ( -75.40625000204838102, 29.18810118750000271, 4.741568889096522788E-15 ) ) ;
#5158 = COLOUR_RGB ( '',0.8941176470588234615, 0.8941176470588234615, 0.8941176470588234615 ) ;
#5159 = DIRECTION ( 'NONE',  ( -1.000000000000000000, 0.000000000000000000, 0.000000000000000000 ) ) ;
#5160 = DIRECTION ( 'NONE',  ( -1.000000000000000000, -0.000000000000000000, -0.000000000000000000 ) ) ;
#5161 = LINE ( 'NONE', #10593, #7883 ) ;
#5162 = AXIS2_PLACEMENT_3D ( 'NONE', #867, #11829, #7360 ) ;
#5163 = CARTESIAN_POINT ( 'NONE',  ( -78.21875000204839523, 36.74823131438024859, -18.25176868561973720 ) ) ;
#5164 = CARTESIAN_POINT ( 'NONE',  ( -80.00000000000000000, 54.99999999999999289, 3.371917797062584654E-06 ) ) ;
#5165 = VECTOR ( 'NONE', #585, 1000.000000000000000 ) ;
#5166 = ORIENTED_EDGE ( 'NONE', *, *, #365, .F. ) ;
#5167 = DIRECTION ( 'NONE',  ( 0.000000000000000000, 0.000000000000000000, -1.000000000000000000 ) ) ;
#5168 = ORIENTED_EDGE ( 'NONE', *, *, #3309, .T. ) ;
#5169 = EDGE_CURVE ( 'NONE', #6748, #8286, #7840, .T. ) ;
#5170 = CARTESIAN_POINT ( 'NONE',  ( -39.66652693873400182, 55.00025670080164275, -7.011456267774554441 ) ) ;
#5171 = DIRECTION ( 'NONE',  ( -1.000000000000000000, 0.000000000000000000, 0.000000000000000000 ) ) ;
#5172 = CYLINDRICAL_SURFACE ( 'NONE', #6707, 24.99999999999999645 ) ;
#5173 = CARTESIAN_POINT ( 'NONE',  ( 47.00000000000000000, 50.00000000000000000, 0.000000000000000000 ) ) ;
#5174 = CIRCLE ( 'NONE', #10693, 1.500000000000001332 ) ;
#5175 = CARTESIAN_POINT ( 'NONE',  ( 20.06119547431871908, 75.62460108169236150, -7.685737028377098490 ) ) ;
#5176 = CARTESIAN_POINT ( 'NONE',  ( -72.96875000204838102, 73.25176868561975141, 18.25176868561974075 ) ) ;
#5177 = EDGE_LOOP ( 'NONE', ( #11401, #7432, #7136, #2356 ) ) ;
#5178 = CARTESIAN_POINT ( 'NONE',  ( -78.12500000204838102, 29.18810118750000626, -10.69163855873949309 ) ) ;
#5179 = CARTESIAN_POINT ( 'NONE',  ( -78.00000000000001421, 67.72792206135787296, -2.742637315201482462 ) ) ;
#5180 = AXIS2_PLACEMENT_3D ( 'NONE', #1992, #10131, #8289 ) ;
#5181 = DIRECTION ( 'NONE',  ( -1.000000000000000000, -0.000000000000000000, -0.000000000000000000 ) ) ;
#5182 = CARTESIAN_POINT ( 'NONE',  ( 6.461783816738637221, 54.99547691306821662, -0.0002561227516112092638 ) ) ;
#5183 = DIRECTION ( 'NONE',  ( 1.000000000000000000, 0.000000000000000000, 0.000000000000000000 ) ) ;
#5184 = FACE_OUTER_BOUND ( 'NONE', #10846, .T. ) ;
#5185 = ADVANCED_FACE ( 'NONE', ( #6342, #9973 ), #6699, .F. ) ;
#5186 = VECTOR ( 'NONE', #1691, 1000.000000000000000 ) ;
#5187 = ORIENTED_EDGE ( 'NONE', *, *, #8591, .T. ) ;
#5188 = CARTESIAN_POINT ( 'NONE',  ( -80.00000000000001421, 67.72792206135787296, 14.22792543327562775 ) ) ;
#5189 = CIRCLE ( 'NONE', #3652, 1.500000000000001332 ) ;
#5190 = CARTESIAN_POINT ( 'NONE',  ( -27.52231952827322559, 42.10572610250680015, 16.77759997522909785 ) ) ;
#5191 = ORIENTED_EDGE ( 'NONE', *, *, #9736, .F. ) ;
#5192 = CARTESIAN_POINT ( 'NONE',  ( -20.07074684291900368, 64.90603024148451539, 18.53632013344132545 ) ) ;
#5193 = CARTESIAN_POINT ( 'NONE',  ( -21.66480673580358385, 60.36362435138872229, 12.94784811284827519 ) ) ;
#5194 = CARTESIAN_POINT ( 'NONE',  ( -78.87500000204838102, 65.69163855873949842, 25.81189881250000440 ) ) ;
#5195 = VECTOR ( 'NONE', #11554, 1000.000000000000000 ) ;
#5196 = VECTOR ( 'NONE', #2820, 1000.000000000000000 ) ;
#5197 = ORIENTED_EDGE ( 'NONE', *, *, #3187, .F. ) ;
#5198 = CARTESIAN_POINT ( 'NONE',  ( -76.90625000204838102, 29.18810118750000271, 4.741568889096522788E-15 ) ) ;
#5199 = CARTESIAN_POINT ( 'NONE',  ( -20.00000000000003197, -57.00000000000000000, 5.000000000000000000 ) ) ;
#5200 = EDGE_CURVE ( 'NONE', #3047, #7152, #6636, .T. ) ;
#5201 = CARTESIAN_POINT ( 'NONE',  ( 14.99999999999999645, -30.00000000000000000, 10.00000000000000000 ) ) ;
#5202 = AXIS2_PLACEMENT_3D ( 'NONE', #34, #7199, #5505 ) ;
#5203 = CARTESIAN_POINT ( 'NONE',  ( 16.81209710897601894, 55.32596159299130534, 5.000262235126429644 ) ) ;
#5204 = CIRCLE ( 'NONE', #1563, 5.000000000000000888 ) ;
#5205 = CARTESIAN_POINT ( 'NONE',  ( -39.89001230141098375, 51.48114101346921245, -6.100591306325558349 ) ) ;
#5206 = EDGE_LOOP ( 'NONE', ( #2449, #10266, #3809, #5054 ) ) ;
#5207 = CARTESIAN_POINT ( 'NONE',  ( 7.391719151893840767, 34.79510180625957361, 6.140032301524222191 ) ) ;
#5208 = DIRECTION ( 'NONE',  ( 1.000000000000000000, -0.000000000000000000, -0.000000000000000000 ) ) ;
#5209 = ADVANCED_FACE ( 'NONE', ( #5673, #2969 ), #262, .F. ) ;
#5210 = CARTESIAN_POINT ( 'NONE',  ( -78.00000000000002842, 38.02943725152282184, 1.500003371917797867 ) ) ;
#5211 = CARTESIAN_POINT ( 'NONE',  ( -3.000000000000000000, 0.000000000000000000, -3.482085714285714229 ) ) ;
#5212 = CARTESIAN_POINT ( 'NONE',  ( -75.21875000204839523, 29.18810118750000271, 4.741568889096522788E-15 ) ) ;
#5213 = ORIENTED_EDGE ( 'NONE', *, *, #4284, .F. ) ;
#5214 = CARTESIAN_POINT ( 'NONE',  ( -73.15625000409677625, 30.00000000000000355, -10.35533905932738108 ) ) ;
#5215 = FACE_OUTER_BOUND ( 'NONE', #5374, .T. ) ;
#5216 = FACE_BOUND ( 'NONE', #2102, .T. ) ;
#5217 = ADVANCED_FACE ( 'NONE', ( #7532 ), #9741, .T. ) ;
#5218 = CARTESIAN_POINT ( 'NONE',  ( -19.63602748969081446, 62.08618401115764129, 19.80343740535094099 ) ) ;
#5219 = EDGE_CURVE ( 'NONE', #10233, #1659, #10268, .T. ) ;
#5220 = ORIENTED_EDGE ( 'NONE', *, *, #9346, .F. ) ;
#5221 = CARTESIAN_POINT ( 'NONE',  ( -75.68750000204838102, 44.30836144126052289, 25.81189881250000795 ) ) ;
#5222 = CARTESIAN_POINT ( 'NONE',  ( -66.03853052622707764, 51.69700120711628699, 3.767903919035947347 ) ) ;
#5223 = DIRECTION ( 'NONE',  ( 0.000000000000000000, 0.000000000000000000, -1.000000000000000000 ) ) ;
#5224 = EDGE_CURVE ( 'NONE', #7962, #7402, #1015, .T. ) ;
#5225 = CARTESIAN_POINT ( 'NONE',  ( -30.67054324275970600, 35.57292846186890500, 8.046485333435041909 ) ) ;
#5226 = CARTESIAN_POINT ( 'NONE',  ( -77.75000000000000000, 55.00000000000000000, 24.99999999999999645 ) ) ;
#5227 = CARTESIAN_POINT ( 'NONE',  ( -75.40625000204838102, 29.18810118750000271, 4.741568889096522788E-15 ) ) ;
#5228 = DIRECTION ( 'NONE',  ( -1.000000000000000000, 0.000000000000000000, 0.000000000000000000 ) ) ;
#5229 = ORIENTED_EDGE ( 'NONE', *, *, #10606, .F. ) ;
#5230 = EDGE_CURVE ( 'NONE', #8109, #7013, #3204, .T. ) ;
#5231 = CARTESIAN_POINT ( 'NONE',  ( -80.00000000000000000, 55.00000000000000000, 0.000000000000000000 ) ) ;
#5232 = ORIENTED_EDGE ( 'NONE', *, *, #2211, .T. ) ;
#5233 = CARTESIAN_POINT ( 'NONE',  ( -30.62461364447335299, 47.99170624137034480, -0.3444639498507808262 ) ) ;
#5234 = FACE_OUTER_BOUND ( 'NONE', #7001, .T. ) ;
#5235 = CARTESIAN_POINT ( 'NONE',  ( -80.00000000000002842, 38.02943725152282184, 1.500003371917797867 ) ) ;
#5236 = CARTESIAN_POINT ( 'NONE',  ( -20.00000000000003197, -63.00000000000000000, -5.000000000000000000 ) ) ;
#5237 = CARTESIAN_POINT ( 'NONE',  ( 21.03141440724603228, 76.42803413576605465, 5.034331618923938656 ) ) ;
#5238 = CARTESIAN_POINT ( 'NONE',  ( 5.000000000000000000, 1.947085426416880649, -5.900379292880307602 ) ) ;
#5239 = VERTEX_POINT ( 'NONE', #5235 ) ;
#5240 = CARTESIAN_POINT ( 'NONE',  ( -74.93750000204839523, 44.30836144126050158, -25.81189881249999374 ) ) ;
#5241 = CARTESIAN_POINT ( 'NONE',  ( 14.99999999999999645, -30.00000000000000000, 10.00000000000000000 ) ) ;
#5242 = UNCERTAINTY_MEASURE_WITH_UNIT (LENGTH_MEASURE( 1.000000000000000082E-05 ), #6220, 'distance_accuracy_value', 'NONE');
#5243 = FACE_OUTER_BOUND ( 'NONE', #8962, .T. ) ;
#5244 = CARTESIAN_POINT ( 'NONE',  ( -12.90719201245152270, 54.97644505888057154, -0.01153927764518185815 ) ) ;
#5245 = DIRECTION ( 'NONE',  ( 1.000000000000000000, 0.000000000000000000, 0.000000000000000000 ) ) ;
#5246 = CARTESIAN_POINT ( 'NONE',  ( -75.00000000000000000, 29.54384304976292697, -0.6381725101535358213 ) ) ;
#5247 = VERTEX_POINT ( 'NONE', #8827 ) ;
#5248 = CARTESIAN_POINT ( 'NONE',  ( -80.00000000000001421, 42.27207793864211283, -14.22791868944003646 ) ) ;
#5249 = CIRCLE ( 'NONE', #7739, 2.981862520314375153 ) ;
#5250 = CARTESIAN_POINT ( 'NONE',  ( -56.32961277634869646, 69.86611656190129338, 14.86520567151240080 ) ) ;
#5251 = ORIENTED_EDGE ( 'NONE', *, *, #4162, .F. ) ;
#5252 = CARTESIAN_POINT ( 'NONE',  ( -55.96940532477286467, 69.12455838185616130, 15.58340920153898956 ) ) ;
#5253 = CARTESIAN_POINT ( 'NONE',  ( -53.16357022681673783, 68.79221833313241063, 2.747526514237220052 ) ) ;
#5254 = CARTESIAN_POINT ( 'NONE',  ( -77.37500000204838102, 65.69163855873949842, 25.81189881250000440 ) ) ;
#5255 = VERTEX_POINT ( 'NONE', #385 ) ;
#5256 = CARTESIAN_POINT ( 'NONE',  ( -77.84375000204839523, 73.25176868561975141, -18.25176868561974430 ) ) ;
#5257 = DIRECTION ( 'NONE',  ( 0.000000000000000000, 0.000000000000000000, -1.000000000000000000 ) ) ;
#5258 =( NAMED_UNIT ( * ) PLANE_ANGLE_UNIT ( ) SI_UNIT ( $, .RADIAN. ) );
#5259 = EDGE_CURVE ( 'NONE', #10459, #3587, #2670, .T. ) ;
#5260 = FACE_OUTER_BOUND ( 'NONE', #5282, .T. ) ;
#5261 = CARTESIAN_POINT ( 'NONE',  ( 24.97984200873575489, 59.96742995076570537, 0.6563446142137170369 ) ) ;
#5262 = CARTESIAN_POINT ( 'NONE',  ( 7.240609414712229963, 54.98725137911733896, 0.01040343736786853227 ) ) ;
#5263 = ORIENTED_EDGE ( 'NONE', *, *, #11755, .T. ) ;
#5264 = CARTESIAN_POINT ( 'NONE',  ( -8.636027272868737725, 70.58382813124079291, -14.12485756978424334 ) ) ;
#5265 = DIRECTION ( 'NONE',  ( -1.000000000000000000, -0.000000000000000000, -0.000000000000000000 ) ) ;
#5266 = DIRECTION ( 'NONE',  ( 0.000000000000000000, 0.000000000000000000, 1.000000000000000000 ) ) ;
#5267 = CARTESIAN_POINT ( 'NONE',  ( -78.00000000000001421, 67.72792206135787296, 14.22792543327562775 ) ) ;
#5268 = DIRECTION ( 'NONE',  ( 1.000000000000000000, 6.033820786006286457E-17, 0.000000000000000000 ) ) ;
#5269 = ORIENTED_EDGE ( 'NONE', *, *, #6814, .F. ) ;
#5270 = CARTESIAN_POINT ( 'NONE',  ( -75.68750000409677625, 72.67766952966368876, -17.67766952966368876 ) ) ;
#5271 = DIRECTION ( 'NONE',  ( -0.000000000000000000, -0.000000000000000000, -1.000000000000000000 ) ) ;
#5272 = FACE_BOUND ( 'NONE', #10636, .T. ) ;
#5273 = CARTESIAN_POINT ( 'NONE',  ( -40.03064391692543467, 53.96877717286832876, -20.99202776130344361 ) ) ;
#5274 = ORIENTED_EDGE ( 'NONE', *, *, #4187, .T. ) ;
#5275 = DIRECTION ( 'NONE',  ( -1.000000000000000000, 0.000000000000000000, 0.000000000000000000 ) ) ;
#5276 = DIRECTION ( 'NONE',  ( 0.000000000000000000, 0.000000000000000000, -1.000000000000000000 ) ) ;
#5277 = CARTESIAN_POINT ( 'NONE',  ( -80.00000000000001421, 59.24264068711928388, -14.22791868944003646 ) ) ;
#5278 = DIRECTION ( 'NONE',  ( 1.000000000000000000, 0.000000000000000000, 0.000000000000000000 ) ) ;
#5279 = DIRECTION ( 'NONE',  ( 0.000000000000000000, 1.000000000000000000, 0.000000000000000000 ) ) ;
#5280 = CARTESIAN_POINT ( 'NONE',  ( -75.96875000204839523, 73.25176868561975141, 18.25176868561974075 ) ) ;
#5281 = CARTESIAN_POINT ( 'NONE',  ( -78.00000000000001421, 54.99999999999998579, -9.985278002320759683 ) ) ;
#5282 = EDGE_LOOP ( 'NONE', ( #6834, #7893, #10443, #10371 ) ) ;
#5283 = LINE ( 'NONE', #11676, #5195 ) ;
#5284 = ORIENTED_EDGE ( 'NONE', *, *, #11785, .T. ) ;
#5285 = CARTESIAN_POINT ( 'NONE',  ( -59.20813656377777079, 53.97164354997492808, 6.936260356707947494 ) ) ;
#5286 = EDGE_CURVE ( 'NONE', #541, #7264, #8789, .T. ) ;
#5287 = DIRECTION ( 'NONE',  ( 0.000000000000000000, 1.000000000000000000, 0.000000000000000000 ) ) ;
#5288 = CARTESIAN_POINT ( 'NONE',  ( 2.074714256722481220, -4.575665857285988736, -6.089444439476605631 ) ) ;
#5289 = CIRCLE ( 'NONE', #103, 2.500000000000000000 ) ;
#5290 = CARTESIAN_POINT ( 'NONE',  ( -78.00000000000001421, 59.24264068711928388, -14.22791868944003646 ) ) ;
#5291 = CARTESIAN_POINT ( 'NONE',  ( 0.000000000000000000, 0.000000000000000000, 0.000000000000000000 ) ) ;
#5292 = ORIENTED_EDGE ( 'NONE', *, *, #1076, .T. ) ;
#5293 = AXIS2_PLACEMENT_3D ( 'NONE', #2109, #4876, #8526 ) ;
#5294 = DIRECTION ( 'NONE',  ( 0.000000000000000000, 0.000000000000000000, 1.000000000000000000 ) ) ;
#5295 = ADVANCED_FACE ( 'NONE', ( #3147 ), #5913, .T. ) ;
#5296 = CARTESIAN_POINT ( 'NONE',  ( -75.40625000204839523, 36.74823131438026280, 18.25176868561974786 ) ) ;
#5297 = EDGE_CURVE ( 'NONE', #642, #10867, #9494, .T. ) ;
#5298 = FACE_OUTER_BOUND ( 'NONE', #9878, .T. ) ;
#5299 = DIRECTION ( 'NONE',  ( 1.000000000000000000, 0.000000000000000000, 0.000000000000000000 ) ) ;
#5300 = CARTESIAN_POINT ( 'NONE',  ( -17.75699671169975957, 54.99635662262475222, -0.009584463525143764942 ) ) ;
#5301 =( LENGTH_UNIT ( ) NAMED_UNIT ( * ) SI_UNIT ( .MILLI., .METRE. ) );
#5302 = LINE ( 'NONE', #8056, #5675 ) ;
#5303 = AXIS2_PLACEMENT_3D ( 'NONE', #1001, #10099, #4660 ) ;
#5304 = EDGE_LOOP ( 'NONE', ( #4511, #10915 ) ) ;
#5305 = FACE_OUTER_BOUND ( 'NONE', #821, .T. ) ;
#5306 = CARTESIAN_POINT ( 'NONE',  ( -20.00000000000003197, -57.00000000000000000, 5.000000000000000000 ) ) ;
#5307 = ORIENTED_EDGE ( 'NONE', *, *, #4225, .F. ) ;
#5308 = CARTESIAN_POINT ( 'NONE',  ( -57.39118702654079129, 64.93227794977589440, 18.59917511543459767 ) ) ;
#5309 = CARTESIAN_POINT ( 'NONE',  ( -79.34375000204839523, 73.25176868561975141, -18.25176868561974430 ) ) ;
#5310 = VECTOR ( 'NONE', #11588, 1000.000000000000000 ) ;
#5311 = CIRCLE ( 'NONE', #4150, 9.999999999999987566 ) ;
#5312 = ORIENTED_EDGE ( 'NONE', *, *, #6847, .F. ) ;
#5313 = CARTESIAN_POINT ( 'NONE',  ( -75.50000000204840944, 29.18810118750000981, 10.69163855873950020 ) ) ;
#5314 = CARTESIAN_POINT ( 'NONE',  ( 24.18742635297404675, 76.02379904146428657, 2.751050496637376774 ) ) ;
#5315 =( NAMED_UNIT ( * ) SI_UNIT ( $, .STERADIAN. ) SOLID_ANGLE_UNIT ( ) );
#5316 = ADVANCED_FACE ( 'NONE', ( #4271, #1510 ), #5172, .T. ) ;
#5317 = CARTESIAN_POINT ( 'NONE',  ( -20.00000000000003197, -63.00000000000000000, -5.000000000000000000 ) ) ;
#5318 = CARTESIAN_POINT ( 'NONE',  ( 2.500000000000000000, 0.000000000000000000, -0.3755037691048591086 ) ) ;
#5319 = CARTESIAN_POINT ( 'NONE',  ( 2.461783834978326091, 54.99737575019351254, -0.0002517746684140311744 ) ) ;
#5320 = ORIENTED_EDGE ( 'NONE', *, *, #6841, .T. ) ;
#5321 = CARTESIAN_POINT ( 'NONE',  ( -13.81096152673235800, 76.02210280262706021, 2.745652712408400031 ) ) ;
#5322 = CARTESIAN_POINT ( 'NONE',  ( 2.003855453843550460, 35.57695044197526357, -8.044733130177707636 ) ) ;
#5323 = DIRECTION ( 'NONE',  ( 0.000000000000000000, 0.000000000000000000, 1.000000000000000000 ) ) ;
#5324 = CARTESIAN_POINT ( 'NONE',  ( -83.00000000000000000, 55.00000000000000000, 0.000000000000000000 ) ) ;
#5325 = APPLICATION_CONTEXT ( 'automotive_design' ) ;
#5326 = CARTESIAN_POINT ( 'NONE',  ( -78.00000000000002842, 54.99999999999998579, 16.97056612039490986 ) ) ;
#5327 = ORIENTED_EDGE ( 'NONE', *, *, #5224, .T. ) ;
#5328 = CYLINDRICAL_SURFACE ( 'NONE', #8440, 1.500000000000000000 ) ;
#5329 = CARTESIAN_POINT ( 'NONE',  ( -78.00000000000001421, 59.24264068711928388, -12.72791868944003824 ) ) ;
#5330 = CARTESIAN_POINT ( 'NONE',  ( -63.67978690865925984, 51.02815575133915615, 3.054710809982001507 ) ) ;
#5331 = VECTOR ( 'NONE', #9283, 1000.000000000000000 ) ;
#5332 = CARTESIAN_POINT ( 'NONE',  ( -61.63584152524990145, 46.00569487729882212, 19.01260273971552905 ) ) ;
#5333 = EDGE_LOOP ( 'NONE', ( #2680, #1018, #8123, #6213 ) ) ;
#5334 = DIRECTION ( 'NONE',  ( 1.000000000000000000, 0.000000000000000000, 0.000000000000000000 ) ) ;
#5335 = ADVANCED_FACE ( 'NONE', ( #4952 ), #9354, .F. ) ;
#5336 = CARTESIAN_POINT ( 'NONE',  ( -56.32252171033144350, 58.97418346094907804, 3.051949254714778625 ) ) ;
#5337 = ORIENTED_EDGE ( 'NONE', *, *, #9466, .F. ) ;
#5338 = DIRECTION ( 'NONE',  ( 0.9986295347545739443, -0.05233595624294389015, 6.409306129323724811E-18 ) ) ;
#5339 = CARTESIAN_POINT ( 'NONE',  ( 6.681748455246894203, 50.66235202709670915, 2.508378333353272982 ) ) ;
#5340 = EDGE_CURVE ( 'NONE', #3514, #9870, #7573, .T. ) ;
#5341 = CARTESIAN_POINT ( 'NONE',  ( -77.18750000204838102, 44.30836144126053000, 25.81189881250000795 ) ) ;
#5342 = CARTESIAN_POINT ( 'NONE',  ( -75.78125000204838102, 55.00000000000000000, 25.81189881249999729 ) ) ;
#5343 = EDGE_LOOP ( 'NONE', ( #8868, #6022, #9585, #3657 ) ) ;
#5344 = CARTESIAN_POINT ( 'NONE',  ( 0.000000000000000000, 110.0000000000000000, 27.53333900685068869 ) ) ;
#5345 = ORIENTED_EDGE ( 'NONE', *, *, #5790, .T. ) ;
#5346 = CARTESIAN_POINT ( 'NONE',  ( -3.016088031971444039, 55.65411387417407951, -4.967671222318850610 ) ) ;
#5347 = CIRCLE ( 'NONE', #917, 1.500000000000001332 ) ;
#5348 = CARTESIAN_POINT ( 'NONE',  ( -13.53949924236008862, 68.61239594966130539, 3.656398761500181838 ) ) ;
#5349 = CYLINDRICAL_SURFACE ( 'NONE', #592, 5.249999999999998224 ) ;
#5350 = CARTESIAN_POINT ( 'NONE',  ( -1.734723475976807094E-14, -5.773502691896260863, -5.653418012614792154 ) ) ;
#5351 = CARTESIAN_POINT ( 'NONE',  ( 0.000000000000000000, 0.000000000000000000, -2.103846626247716234 ) ) ;
#5352 = VECTOR ( 'NONE', #753, 1000.000000000000000 ) ;
#5353 = DIRECTION ( 'NONE',  ( -1.000000000000000000, -0.000000000000000000, -0.000000000000000000 ) ) ;
#5354 = ORIENTED_EDGE ( 'NONE', *, *, #3166, .F. ) ;
#5355 = CARTESIAN_POINT ( 'NONE',  ( -75.50000000204840944, 44.30836144126053000, 25.81189881250000795 ) ) ;
#5356 = ADVANCED_FACE ( 'NONE', ( #3852 ), #739, .F. ) ;
#5357 = DIRECTION ( 'NONE',  ( -1.000000000000000000, 0.000000000000000000, 0.000000000000000000 ) ) ;
#5358 = CARTESIAN_POINT ( 'NONE',  ( 0.000000000000000000, 0.000000000000000000, -6.099999999999999645 ) ) ;
#5359 = CARTESIAN_POINT ( 'NONE',  ( -28.24307224120747861, 54.99071020490737993, 0.002851684764032580855 ) ) ;
#5360 = AXIS2_PLACEMENT_3D ( 'NONE', #9259, #10034, #929 ) ;
#5361 = DIRECTION ( 'NONE',  ( 0.000000000000000000, 0.3830907810419885706, 0.9237106979355818037 ) ) ;
#5362 = CARTESIAN_POINT ( 'NONE',  ( 0.000000000000000000, -17.82799999999998875, 0.000000000000000000 ) ) ;
#5363 = VERTEX_POINT ( 'NONE', #5651 ) ;
#5364 = CARTESIAN_POINT ( 'NONE',  ( -22.84604256752122708, 53.39459927986023757, 4.746710467859072580 ) ) ;
#5365 = CARTESIAN_POINT ( 'NONE',  ( -54.88146047731135013, 73.03677976846768161, 10.81065700633557825 ) ) ;
#5366 = EDGE_LOOP ( 'NONE', ( #6302, #5984, #7721, #7053 ) ) ;
#5367 = CARTESIAN_POINT ( 'NONE',  ( -43.40408007066994145, 61.10253656447230952, -20.11177873753167589 ) ) ;
#5368 = CARTESIAN_POINT ( 'NONE',  ( -75.03125000204838102, 55.00000000000000000, -25.81189881249999729 ) ) ;
#5369 = EDGE_LOOP ( 'NONE', ( #3956, #9098, #3145, #2155 ) ) ;
#5370 = EDGE_CURVE ( 'NONE', #8222, #9107, #11265, .T. ) ;
#5371 = CARTESIAN_POINT ( 'NONE',  ( -72.21875000204838102, 36.74823131438024859, -18.25176868561973720 ) ) ;
#5372 = CARTESIAN_POINT ( 'NONE',  ( 17.18896242946999919, 60.50854855881860317, 20.47421955154796436 ) ) ;
#5373 =( NAMED_UNIT ( * ) PLANE_ANGLE_UNIT ( ) SI_UNIT ( $, .RADIAN. ) );
#5374 = EDGE_LOOP ( 'NONE', ( #4639, #10024, #2996, #8819 ) ) ;
#5375 = AXIS2_PLACEMENT_3D ( 'NONE', #3018, #9299, #6686 ) ;
#5376 = CARTESIAN_POINT ( 'NONE',  ( -78.00000000000000000, 55.00000000000000000, 0.000000000000000000 ) ) ;
#5377 = CARTESIAN_POINT ( 'NONE',  ( -75.00000000000000000, 55.00000000000000000, 0.000000000000000000 ) ) ;
#5378 = CARTESIAN_POINT ( 'NONE',  ( -57.00013066340230949, 59.95461989290591731, 4.954166194309457261 ) ) ;
#5379 = EDGE_LOOP ( 'NONE', ( #7275, #5166, #6073, #4764 ) ) ;
#5380 = CARTESIAN_POINT ( 'NONE',  ( -2.144294859876037851, 49.49184188862220424, -20.47260631371810291 ) ) ;
#5381 = VECTOR ( 'NONE', #6912, 1000.000000000000000 ) ;
#5382 = CIRCLE ( 'NONE', #3848, 1.500000000000001332 ) ;
#5383 = CARTESIAN_POINT ( 'NONE',  ( -41.16026710375170694, 50.89060761561553647, -20.69263693287480521 ) ) ;
#5384 = CARTESIAN_POINT ( 'NONE',  ( -75.00000000000000000, 55.00000000000000000, 0.000000000000000000 ) ) ;
#5385 = CARTESIAN_POINT ( 'NONE',  ( -75.68750000000005684, 37.32233047033638940, -17.67766952966360705 ) ) ;
#5386 = CARTESIAN_POINT ( 'NONE',  ( -4.180704885107416224, -3.359771601077114589, -5.901655677627838159 ) ) ;
#5387 = ORIENTED_EDGE ( 'NONE', *, *, #2723, .T. ) ;
#5388 = CARTESIAN_POINT ( 'NONE',  ( -71.09375000409677625, 80.00000000000001421, -10.35533905932737753 ) ) ;
#5389 = FACE_OUTER_BOUND ( 'NONE', #2733, .T. ) ;
#5390 = CARTESIAN_POINT ( 'NONE',  ( 39.99999999999999289, 55.00000000000000000, -24.99999999999999645 ) ) ;
#5391 = ORIENTED_EDGE ( 'NONE', *, *, #3187, .T. ) ;
#5392 = CIRCLE ( 'NONE', #3667, 5.000000000000000000 ) ;
#5393 = DIRECTION ( 'NONE',  ( 0.000000000000000000, 1.000000000000000000, 0.000000000000000000 ) ) ;
#5394 = VECTOR ( 'NONE', #4982, 1000.000000000000000 ) ;
#5395 = DIRECTION ( 'NONE',  ( 0.000000000000000000, 1.000000000000000000, 0.000000000000000000 ) ) ;
#5396 = ORIENTED_EDGE ( 'NONE', *, *, #9953, .T. ) ;
#5397 = CYLINDRICAL_SURFACE ( 'NONE', #5515, 9.999999999999987566 ) ;
#5398 = CARTESIAN_POINT ( 'NONE',  ( -20.00000000000003197, -57.00000000000000000, 5.000000000000000000 ) ) ;
#5399 = CARTESIAN_POINT ( 'NONE',  ( -74.28125000204838102, 55.00000000000000000, 25.81189881249999729 ) ) ;
#5400 = CIRCLE ( 'NONE', #14, 1.500000000000001332 ) ;
#5401 = CARTESIAN_POINT ( 'NONE',  ( -77.75000000204839523, 80.81189881250001861, -10.69163855873949132 ) ) ;
#5402 = EDGE_LOOP ( 'NONE', ( #6319, #10792 ) ) ;
#5403 = CARTESIAN_POINT ( 'NONE',  ( -75.78125000204839523, 73.25176868561975141, 18.25176868561974075 ) ) ;
#5404 = VERTEX_POINT ( 'NONE', #6618 ) ;
#5405 = CARTESIAN_POINT ( 'NONE',  ( 3.983988775803998905, 50.66121500187745852, -2.506212315349996445 ) ) ;
#5406 = CARTESIAN_POINT ( 'NONE',  ( 10.53956211717208014, 43.78843572598016465, 8.622155805075909285 ) ) ;
#5407 = CARTESIAN_POINT ( 'NONE',  ( -76.25000000204838102, 65.69163855873948421, -25.81189881250000084 ) ) ;
#5408 = EDGE_CURVE ( 'NONE', #3592, #1675, #7656, .T. ) ;
#5409 = CARTESIAN_POINT ( 'NONE',  ( 1.443735181952764846, -4.939961795957305668, -6.018341802876223667 ) ) ;
#5410 = CARTESIAN_POINT ( 'NONE',  ( -2.500000000000000000, 3.061616997868383141E-16, -1.239675197676287643 ) ) ;
#5411 = VERTEX_POINT ( 'NONE', #2269 ) ;
#5412 = CARTESIAN_POINT ( 'NONE',  ( -76.15625000409677625, 30.00000000000000355, -10.35533905932738108 ) ) ;
#5413 = CARTESIAN_POINT ( 'NONE',  ( -75.78125000409680467, 65.35533905932737753, -24.99999999999999645 ) ) ;
#5414 = EDGE_CURVE ( 'NONE', #6251, #8998, #9289, .T. ) ;
#5415 = DIRECTION ( 'NONE',  ( 0.000000000000000000, 1.000000000000000000, 0.000000000000000000 ) ) ;
#5416 = CARTESIAN_POINT ( 'NONE',  ( 3.000000000000000000, 3.673940397442059868E-16, -3.482085714285714229 ) ) ;
#5417 = CARTESIAN_POINT ( 'NONE',  ( -50.99787495343821320, 55.00280540214748726, 0.001329527542247992220 ) ) ;
#5418 = APPLICATION_PROTOCOL_DEFINITION ( 'draft international standard', 'automotive_design', 1998, #2098 ) ;
#5419 = DIRECTION ( 'NONE',  ( 0.000000000000000000, 1.000000000000000000, 0.000000000000000000 ) ) ;
#5420 = DIRECTION ( 'NONE',  ( -0.5000000000000009992, -0.8660254037844380415, 0.000000000000000000 ) ) ;
#5421 = ORIENTED_EDGE ( 'NONE', *, *, #3201, .F. ) ;
#5422 = CARTESIAN_POINT ( 'NONE',  ( -61.88037028687247698, 51.91449295574040690, 20.80032498971814192 ) ) ;
#5423 = VERTEX_POINT ( 'NONE', #9236 ) ;
#5424 = CARTESIAN_POINT ( 'NONE',  ( -60.33823637602682766, 55.00059828005016982, 21.02834956124393884 ) ) ;
#5425 = CARTESIAN_POINT ( 'NONE',  ( -79.15625000204839523, 73.25176868561975141, -18.25176868561974430 ) ) ;
#5426 = ADVANCED_FACE ( 'NONE', ( #10469 ), #2954, .F. ) ;
#5427 = ORIENTED_EDGE ( 'NONE', *, *, #6539, .T. ) ;
#5428 = CARTESIAN_POINT ( 'NONE',  ( -76.43750000204838102, 65.69163855873948421, -25.81189881250000440 ) ) ;
#5429 = CARTESIAN_POINT ( 'NONE',  ( -11.52239577449127061, 75.97627689174807131, -2.745668057393931161 ) ) ;
#5430 = EDGE_LOOP ( 'NONE', ( #11846, #1590, #1250, #3005 ) ) ;
#5431 = EDGE_CURVE ( 'NONE', #896, #7402, #3175, .T. ) ;
#5432 = ADVANCED_FACE ( 'NONE', ( #9639, #5598, #528, #7517, #7851, #4684, #10246, #9584, #1380, #8336, #11480, #11422, #11138, #245, #3291, #3786, #7455, #1984, #3909, #2044, #2893, #5717, #8689, #6562, #1142, #1085, #4750, #6845, #5042, #471 ), #4128, .T. ) ;
#5433 = LINE ( 'NONE', #4531, #2081 ) ;
#5434 = CARTESIAN_POINT ( 'NONE',  ( -9.795201718507710709, 54.99722681578106886, 0.002449751363073274148 ) ) ;
#5435 = ORIENTED_EDGE ( 'NONE', *, *, #1143, .T. ) ;
#5436 = ADVANCED_FACE ( 'NONE', ( #7138 ), #11724, .F. ) ;
#5437 = CARTESIAN_POINT ( 'NONE',  ( 4.785240962488377825, 34.19851723175345626, -3.085388102356358075 ) ) ;
#5438 = CARTESIAN_POINT ( 'NONE',  ( -42.33720994522852266, 55.00043528610386545, -21.02753041772728437 ) ) ;
#5439 = CARTESIAN_POINT ( 'NONE',  ( 5.000000000000000000, -0.9724665692850897880, -6.058069561147904736 ) ) ;
#5440 = DIRECTION ( 'NONE',  ( 0.000000000000000000, 0.000000000000000000, 1.000000000000000000 ) ) ;
#5441 = AXIS2_PLACEMENT_3D ( 'NONE', #11594, #1488, #5091 ) ;
#5442 = CYLINDRICAL_SURFACE ( 'NONE', #1714, 1.499999999999999556 ) ;
#5443 = ORIENTED_EDGE ( 'NONE', *, *, #72, .F. ) ;
#5444 = CARTESIAN_POINT ( 'NONE',  ( -76.62500000000005684, 79.99999999999991473, -1.530808498934185605E-15 ) ) ;
#5445 = CARTESIAN_POINT ( 'NONE',  ( -48.75936011024216299, 55.01274827867656114, -0.01040309443492500041 ) ) ;
#5446 = CARTESIAN_POINT ( 'NONE',  ( -33.35108528763237956, 50.66059424145658596, -2.505263451482964143 ) ) ;
#5447 = VERTEX_POINT ( 'NONE', #2451 ) ;
#5448 = DIRECTION ( 'NONE',  ( -6.033820786006286457E-17, 1.000000000000000000, 0.000000000000000000 ) ) ;
#5449 = CARTESIAN_POINT ( 'NONE',  ( -70.70219505483254352, 49.99995498154407159, 0.3302917765627791380 ) ) ;
#5450 = EDGE_LOOP ( 'NONE', ( #8877, #7543, #5345, #4625 ) ) ;
#5451 = CARTESIAN_POINT ( 'NONE',  ( -78.00000000000002842, 50.75735931288069480, 2.742644059037076865 ) ) ;
#5452 = DIRECTION ( 'NONE',  ( -1.000000000000000000, -0.000000000000000000, -0.000000000000000000 ) ) ;
#5453 = CARTESIAN_POINT ( 'NONE',  ( 0.000000000000000000, 0.000000000000000000, -0.02539999999999996774 ) ) ;
#5454 = CARTESIAN_POINT ( 'NONE',  ( -2.149629781808683138, 65.58267949266357277, -22.64980306772420349 ) ) ;
#5455 = FACE_OUTER_BOUND ( 'NONE', #1504, .T. ) ;
#5456 =( GEOMETRIC_REPRESENTATION_CONTEXT ( 3 ) GLOBAL_UNCERTAINTY_ASSIGNED_CONTEXT ( ( #7719 ) ) GLOBAL_UNIT_ASSIGNED_CONTEXT ( ( #5301, #2484, #7165 ) ) REPRESENTATION_CONTEXT ( 'NONE', 'WORKASPACE' ) );
#5457 = ORIENTED_EDGE ( 'NONE', *, *, #7340, .F. ) ;
#5458 = CARTESIAN_POINT ( 'NONE',  ( -76.62500000204839523, 29.18810118750000626, -10.69163855873949309 ) ) ;
#5459 = ORIENTED_EDGE ( 'NONE', *, *, #5224, .F. ) ;
#5460 = CARTESIAN_POINT ( 'NONE',  ( 12.37746768708380074, 69.98505844884790861, 20.01803919467661430 ) ) ;
#5461 = CARTESIAN_POINT ( 'NONE',  ( -10.46040627582160099, 68.65766219505340473, -3.675420389180045433 ) ) ;
#5462 = CARTESIAN_POINT ( 'NONE',  ( -76.15625000204839523, 73.25176868561975141, -18.25176868561974430 ) ) ;
#5463 = CARTESIAN_POINT ( 'NONE',  ( -79.25000000000000000, 55.00000000000000000, 24.99999999999999645 ) ) ;
#5464 = MECHANICAL_DESIGN_GEOMETRIC_PRESENTATION_REPRESENTATION (  '', ( #4316 ), #11372 ) ;
#5465 = DIRECTION ( 'NONE',  ( -1.000000000000000000, -0.000000000000000000, -0.000000000000000000 ) ) ;
#5466 = ORIENTED_EDGE ( 'NONE', *, *, #8705, .F. ) ;
#5467 = CARTESIAN_POINT ( 'NONE',  ( 1.648146632868998651, 4.821944789745366222, 4.199965926460685847E-15 ) ) ;
#5468 = CARTESIAN_POINT ( 'NONE',  ( -77.56250000409679046, 37.32233047033631124, -17.67766952966368166 ) ) ;
#5469 =( BOUNDED_CURVE ( )  B_SPLINE_CURVE ( 2, ( #6822, #5919, #8615, #270, #3933, #4062, #6642, #11346, #214 ),
 .UNSPECIFIED., .F., .T. ) 
 B_SPLINE_CURVE_WITH_KNOTS ( ( 3, 2, 2, 2, 3 ),
 ( 0.2500000000000002220, 0.2708333333333335369, 0.2916666666666669627, 0.3125000000000002776, 0.3333333333333335924 ),
 .UNSPECIFIED. ) 
 CURVE ( )  GEOMETRIC_REPRESENTATION_ITEM ( )  RATIONAL_B_SPLINE_CURVE ( ( 0.9999999999999992228, 0.9238795325112875156, 1.000000000000000000, 0.9238795325112867385, 1.000000000000000000, 0.9238795325112867385, 1.000000000000000000, 0.9238795325112857393, 1.000000000000001110 ) ) 
 REPRESENTATION_ITEM ( '' )  );
#5470 = FACE_OUTER_BOUND ( 'NONE', #9660, .T. ) ;
#5471 = CARTESIAN_POINT ( 'NONE',  ( -42.82983869248258912, 55.00187443791501352, -0.004031347153255517880 ) ) ;
#5472 = CARTESIAN_POINT ( 'NONE',  ( -3.965853256712214225, 65.56424026801020943, -19.29796592139343758 ) ) ;
#5473 = AXIS2_PLACEMENT_3D ( 'NONE', #10631, #2262, #8017 ) ;
#5474 = CARTESIAN_POINT ( 'NONE',  ( -8.852116072238684907, 59.49383071322154848, -2.216568777849228677 ) ) ;
#5475 = ORIENTED_EDGE ( 'NONE', *, *, #1032, .F. ) ;
#5476 = CIRCLE ( 'NONE', #3752, 1.500000000000001332 ) ;
#5477 = CARTESIAN_POINT ( 'NONE',  ( -78.00000000000002842, 50.75735931288069480, 5.742644059037076865 ) ) ;
#5478 = ORIENTED_EDGE ( 'NONE', *, *, #899, .T. ) ;
#5479 = CARTESIAN_POINT ( 'NONE',  ( 3.451907635234679361, 34.19915017745972108, -3.085386652995293133 ) ) ;
#5480 = CARTESIAN_POINT ( 'NONE',  ( -73.25000000204838102, 80.81189881250001861, -10.69163855873949132 ) ) ;
#5481 = VECTOR ( 'NONE', #1161, 1000.000000000000114 ) ;
#5482 = EDGE_CURVE ( 'NONE', #9843, #388, #1550, .T. ) ;
#5483 = ORIENTED_EDGE ( 'NONE', *, *, #8211, .F. ) ;
#5484 = CARTESIAN_POINT ( 'NONE',  ( -75.59375000204839523, 36.74823131438026280, 18.25176868561974786 ) ) ;
#5485 = CARTESIAN_POINT ( 'NONE',  ( -17.59602449223222109, 68.34579465778965357, 16.25793134507749826 ) ) ;
#5486 = AXIS2_PLACEMENT_3D ( 'NONE', #10165, #223, #6595 ) ;
#5487 = VERTEX_POINT ( 'NONE', #6062 ) ;
#5488 = CYLINDRICAL_SURFACE ( 'NONE', #9154, 1.500000000000000444 ) ;
#5489 = SHAPE_REPRESENTATION ( 'MAS-170', ( #2775, #277, #6997, #6807, #10027, #4883, #6419, #6238 ), #1623 ) ;
#5490 = CARTESIAN_POINT ( 'NONE',  ( 22.00000000000000711, 54.99999999999999289, 0.000000000000000000 ) ) ;
#5491 = ORIENTED_EDGE ( 'NONE', *, *, #2710, .T. ) ;
#5492 = CARTESIAN_POINT ( 'NONE',  ( -35.52239577659344860, 38.22489504150217243, -12.89214396572665500 ) ) ;
#5493 = VECTOR ( 'NONE', #1482, 1000.000000000000000 ) ;
#5494 = CARTESIAN_POINT ( 'NONE',  ( 0.8268573817076104726, 37.44832105976551873, -11.71822709476406210 ) ) ;
#5495 = CARTESIAN_POINT ( 'NONE',  ( 0.8179331680533001858, 5.301268757141563093, -5.926062401966624371 ) ) ;
#5496 = CARTESIAN_POINT ( 'NONE',  ( 0.000000000000000000, -17.00000000000000000, 0.000000000000000000 ) ) ;
#5497 = AXIS2_PLACEMENT_3D ( 'NONE', #4951, #6578, #7648 ) ;
#5498 = DIRECTION ( 'NONE',  ( 0.8191520442889913545, 1.003171929053524254E-16, -0.5735764363510468256 ) ) ;
#5499 = DIRECTION ( 'NONE',  ( 0.000000000000000000, 0.000000000000000000, -1.000000000000000000 ) ) ;
#5500 = EDGE_CURVE ( 'NONE', #10858, #7962, #4252, .T. ) ;
#5501 = EDGE_LOOP ( 'NONE', ( #2780, #8519, #11205, #6638, #1607, #7694 ) ) ;
#5502 = LINE ( 'NONE', #2859, #1159 ) ;
#5503 = CARTESIAN_POINT ( 'NONE',  ( -27.75939058475275800, 54.99220303251508568, 0.01449020901263564122 ) ) ;
#5504 = CARTESIAN_POINT ( 'NONE',  ( -52.01616715382184708, 59.33866825769318609, 2.506581953018356845 ) ) ;
#5505 = DIRECTION ( 'NONE',  ( 0.000000000000000000, 1.000000000000000000, 0.000000000000000000 ) ) ;
#5506 = VECTOR ( 'NONE', #10965, 1000.000000000000000 ) ;
#5507 = CARTESIAN_POINT ( 'NONE',  ( 8.673617379884035472E-16, 5.773502691896260863, 0.000000000000000000 ) ) ;
#5508 = ADVANCED_FACE ( 'NONE', ( #6117 ), #10818, .F. ) ;
#5509 = ORIENTED_EDGE ( 'NONE', *, *, #2138, .T. ) ;
#5510 = CARTESIAN_POINT ( 'NONE',  ( -8.839809468419982608, 72.54364378520992318, -11.73195350307014273 ) ) ;
#5511 = DIRECTION ( 'NONE',  ( -0.000000000000000000, 0.000000000000000000, -1.000000000000000000 ) ) ;
#5512 = CARTESIAN_POINT ( 'NONE',  ( 20.68040016808398107, 59.84041032842515762, 1.294695803031751247 ) ) ;
#5513 = CARTESIAN_POINT ( 'NONE',  ( -18.39575369641156399, 74.32255031325632899, -15.87762562984429415 ) ) ;
#5514 = CARTESIAN_POINT ( 'NONE',  ( -79.15625000204838102, 80.81189881250000440, -1.580522963032174394E-15 ) ) ;
#5515 = AXIS2_PLACEMENT_3D ( 'NONE', #7086, #8204, #10887 ) ;
#5516 = VERTEX_POINT ( 'NONE', #7911 ) ;
#5517 = CARTESIAN_POINT ( 'NONE',  ( -76.06250000204840944, 80.81189881250001861, -10.69163855873949132 ) ) ;
#5518 = ORIENTED_EDGE ( 'NONE', *, *, #10219, .T. ) ;
#5519 = CARTESIAN_POINT ( 'NONE',  ( 11.01771772720809572, 69.13422207321994506, 20.62759405020127801 ) ) ;
#5520 = CARTESIAN_POINT ( 'NONE',  ( -5.589484852938766402, 61.61028781279477329, -12.37056010730757194 ) ) ;
#5521 = CARTESIAN_POINT ( 'NONE',  ( -75.87500000204838102, 80.81189881250000440, 10.69163855873948243 ) ) ;
#5522 = CARTESIAN_POINT ( 'NONE',  ( -78.00000000000001421, 42.27207793864211283, -12.72791868944003824 ) ) ;
#5523 = DIRECTION ( 'NONE',  ( 0.000000000000000000, -1.000000000000000000, 0.000000000000000000 ) ) ;
#5524 = ORIENTED_EDGE ( 'NONE', *, *, #11792, .F. ) ;
#5525 = CARTESIAN_POINT ( 'NONE',  ( -79.90625000000000000, 65.35533905932737753, -24.99999999999999645 ) ) ;
#5526 = CARTESIAN_POINT ( 'NONE',  ( -72.03125000204839523, 36.74823131438024859, -18.25176868561973720 ) ) ;
#5527 = AXIS2_PLACEMENT_3D ( 'NONE', #688, #4360, #8012 ) ;
#5528 = ADVANCED_FACE ( 'NONE', ( #5389 ), #11775, .F. ) ;
#5529 = DIRECTION ( 'NONE',  ( -1.000000000000000000, -0.000000000000000000, -0.000000000000000000 ) ) ;
#5530 = CARTESIAN_POINT ( 'NONE',  ( -66.57380018018302792, 55.02491533713232030, -0.005784342931633022940 ) ) ;
#5531 = APPLICATION_PROTOCOL_DEFINITION ( 'draft international standard', 'automotive_design', 1998, #1863 ) ;
#5532 = CARTESIAN_POINT ( 'NONE',  ( -20.85448682672772946, 76.28028968605049442, -5.762572995040112112 ) ) ;
#5533 = AXIS2_PLACEMENT_3D ( 'NONE', #2087, #8507, #287 ) ;
#5534 = CARTESIAN_POINT ( 'NONE',  ( -21.68459333372202735, 54.34592763142354244, 4.967663218408093329 ) ) ;
#5535 = AXIS2_PLACEMENT_3D ( 'NONE', #5376, #7242, #10865 ) ;
#5536 = ORIENTED_EDGE ( 'NONE', *, *, #6430, .F. ) ;
#5537 = CARTESIAN_POINT ( 'NONE',  ( -74.18750000409677625, 72.67766952966368876, -17.67766952966368876 ) ) ;
#5538 = ORIENTED_EDGE ( 'NONE', *, *, #3463, .T. ) ;
#5539 = CARTESIAN_POINT ( 'NONE',  ( 19.85574934264614910, 73.36821619702706698, 10.58005382006121131 ) ) ;
#5540 =( BOUNDED_CURVE ( )  B_SPLINE_CURVE ( 2, ( #1854, #3778, #8328, #4452, #1014, #6487, #11741, #4567, #7329, #9947, #9055, #9001, #10840, #3541, #3717, #4677, #7215, #110, #7446, #3664, #6425, #10899, #11008, #2647, #6312, #8217, #7270, #4620, #8274, #891, #832, #1743, #9886, #5407, #5462, #11073, #4504, #5521, #8157, #2764, #11799, #2884, #10116, #10954, #2711, #3604, #6374, #10000, #1795 ),
 .UNSPECIFIED., .F., .T. ) 
 B_SPLINE_CURVE_WITH_KNOTS ( ( 3, 2, 2, 2, 2, 2, 2, 2, 2, 2, 2, 2, 2, 2, 2, 2, 2, 2, 2, 2, 2, 2, 2, 2, 3 ),
 ( 0.000000000000000000, 0.02083333333333333218, 0.04166666666666666435, 0.06250000000000000000, 0.08333333333333332871, 0.1041666666666666713, 0.1250000000000000000, 0.1458333333333333426, 0.1666666666666666574, 0.1875000000000000000, 0.2083333333333333426, 0.2291666666666666574, 0.2500000000000000000, 0.2708333333333333148, 0.2916666666666666852, 0.3125000000000000000, 0.3333333333333333148, 0.3541666666666666852, 0.3750000000000000000, 0.3958333333333333148, 0.4166666666666666852, 0.4375000000000000000, 0.4583333333333333148, 0.4791666666666666852, 0.4827908099017684251 ),
 .UNSPECIFIED. ) 
 CURVE ( )  GEOMETRIC_REPRESENTATION_ITEM ( )  RATIONAL_B_SPLINE_CURVE ( ( 1.000000000000000000, 0.9238795325112867385, 1.000000000000000000, 0.9238795325112867385, 1.000000000000000000, 0.9238795325112867385, 1.000000000000000000, 0.9238795325112867385, 1.000000000000000000, 0.9238795325112867385, 1.000000000000000000, 0.9238795325112867385, 1.000000000000000000, 0.9238795325112867385, 1.000000000000000000, 0.9238795325112867385, 1.000000000000000000, 0.9238795325112867385, 1.000000000000000000, 0.9238795325112867385, 1.000000000000000000, 0.9238795325112867385, 1.000000000000000000, 0.9238795325112867385, 1.000000000000000000, 0.9238795325112867385, 1.000000000000000000, 0.9238795325112867385, 1.000000000000000000, 0.9238795325112867385, 1.000000000000000000, 0.9238795325112867385, 1.000000000000000000, 0.9238795325112867385, 1.000000000000000000, 0.9238795325112867385, 1.000000000000000000, 0.9238795325112867385, 1.000000000000000000, 0.9238795325112867385, 1.000000000000000000, 0.9238795325112867385, 1.000000000000000000, 0.9238795325112867385, 1.000000000000000000, 0.9238795325112867385, 1.000000000000000000, 0.9867581690895038671, 0.9781234062028126841 ) ) 
 REPRESENTATION_ITEM ( '' )  );
#5541 = CARTESIAN_POINT ( 'NONE',  ( -78.12500000204838102, 29.18810118750000626, -10.69163855873949309 ) ) ;
#5542 = AXIS2_PLACEMENT_3D ( 'NONE', #8431, #5746, #3155 ) ;
#5543 = AXIS2_PLACEMENT_3D ( 'NONE', #3656, #7438, #3597 ) ;
#5544 = ORIENTED_EDGE ( 'NONE', *, *, #3019, .T. ) ;
#5545 = ADVANCED_FACE ( 'NONE', ( #3523 ), #11540, .F. ) ;
#5546 = CARTESIAN_POINT ( 'NONE',  ( -75.96875000204839523, 73.25176868561975141, 18.25176868561974075 ) ) ;
#5547 = CARTESIAN_POINT ( 'NONE',  ( -39.16026728571524984, 50.89059911655681390, -20.69167526169209026 ) ) ;
#5548 = CARTESIAN_POINT ( 'NONE',  ( -41.21475901749523274, 58.08538884819615333, -20.80179922188357011 ) ) ;
#5549 = ORIENTED_EDGE ( 'NONE', *, *, #1030, .T. ) ;
#5550 = APPLICATION_CONTEXT ( 'automotive_design' ) ;
#5551 = CARTESIAN_POINT ( 'NONE',  ( 62.44550000000000267, 55.00000000000000000, 0.000000000000000000 ) ) ;
#5552 = CARTESIAN_POINT ( 'NONE',  ( -77.93750000000005684, 72.67766952966363192, 17.67766952966363547 ) ) ;
#5553 = AXIS2_PLACEMENT_3D ( 'NONE', #7361, #2624, #5559 ) ;
#5554 = ORIENTED_EDGE ( 'NONE', *, *, #9679, .F. ) ;
#5555 = CARTESIAN_POINT ( 'NONE',  ( -49.52233824455085909, 75.97792204488571599, -2.745941792655960167 ) ) ;
#5556 = CARTESIAN_POINT ( 'NONE',  ( -26.81096152405270061, 44.41979049410412017, 18.36814973051028588 ) ) ;
#5557 = CARTESIAN_POINT ( 'NONE',  ( 0.000000000000000000, 0.000000000000000000, -5.210428571428570521 ) ) ;
#5558 = DIRECTION ( 'NONE',  ( 0.000000000000000000, 0.000000000000000000, 1.000000000000000000 ) ) ;
#5559 = DIRECTION ( 'NONE',  ( -1.000000000000000000, 0.000000000000000000, 0.000000000000000000 ) ) ;
#5560 = ADVANCED_FACE ( 'NONE', ( #5215 ), #9697, .F. ) ;
#5561 = ORIENTED_EDGE ( 'NONE', *, *, #7905, .T. ) ;
#5562 = DIRECTION ( 'NONE',  ( 0.000000000000000000, 0.000000000000000000, -1.000000000000000000 ) ) ;
#5563 = CARTESIAN_POINT ( 'NONE',  ( -55.57639901084645828, 55.00517665877310236, 0.003022361695382154087 ) ) ;
#5564 = CARTESIAN_POINT ( 'NONE',  ( -61.34696192836374706, 52.49897595166400777, 4.332661177462228785 ) ) ;
#5565 = AXIS2_PLACEMENT_3D ( 'NONE', #5061, #8709, #11385 ) ;
#5566 = DIRECTION ( 'NONE',  ( 1.000000000000000000, 6.033820786006286457E-17, -0.000000000000000000 ) ) ;
#5567 = FACE_OUTER_BOUND ( 'NONE', #9764, .T. ) ;
#5568 = ORIENTED_EDGE ( 'NONE', *, *, #10188, .T. ) ;
#5569 = CARTESIAN_POINT ( 'NONE',  ( 19.52230480204648799, 67.92440004991483704, 16.80766691833610693 ) ) ;
#5570 = CARTESIAN_POINT ( 'NONE',  ( -73.81250000204839523, 29.18810118750000626, -10.69163855873949132 ) ) ;
#5571 = CIRCLE ( 'NONE', #9194, 3.000000000000000000 ) ;
#5572 = DIRECTION ( 'NONE',  ( -1.000000000000000000, -0.000000000000000000, -0.000000000000000000 ) ) ;
#5573 = CARTESIAN_POINT ( 'NONE',  ( 5.513839465024632069, 50.25394865510380527, 1.607139511838376000 ) ) ;
#5574 = CARTESIAN_POINT ( 'NONE',  ( -23.65491598197041156, 78.60782538777030481, -8.235832699802983825 ) ) ;
#5575 = CARTESIAN_POINT ( 'NONE',  ( -75.21875000204839523, 36.74823131438024859, -18.25176868561973720 ) ) ;
#5576 = EDGE_CURVE ( 'NONE', #11822, #3874, #4006, .T. ) ;
#5577 = ORIENTED_EDGE ( 'NONE', *, *, #6690, .F. ) ;
#5578 = ADVANCED_FACE ( 'NONE', ( #3405 ), #3344, .F. ) ;
#5579 = EDGE_CURVE ( 'NONE', #4918, #642, #10314, .T. ) ;
#5580 = FACE_OUTER_BOUND ( 'NONE', #5402, .T. ) ;
#5581 = AXIS2_PLACEMENT_3D ( 'NONE', #1791, #10178, #9163 ) ;
#5582 = ORIENTED_EDGE ( 'NONE', *, *, #2710, .F. ) ;
#5583 = CARTESIAN_POINT ( 'NONE',  ( -19.29698723374914593, 59.72494936439868951, 13.20503860676303098 ) ) ;
#5584 = FACE_OUTER_BOUND ( 'NONE', #940, .T. ) ;
#5585 = CARTESIAN_POINT ( 'NONE',  ( -74.99999999999998579, 72.97359286453712457, -18.15706671146198303 ) ) ;
#5586 = ADVANCED_FACE ( 'NONE', ( #8808 ), #1604, .T. ) ;
#5587 = EDGE_CURVE ( 'NONE', #8286, #6748, #1889, .T. ) ;
#5588 = CYLINDRICAL_SURFACE ( 'NONE', #9901, 1.500000000000000444 ) ;
#5589 = VECTOR ( 'NONE', #7756, 1000.000000000000000 ) ;
#5590 = ORIENTED_EDGE ( 'NONE', *, *, #5576, .T. ) ;
#5591 = PRODUCT_DEFINITION_SHAPE ( 'NONE', 'NONE',  #3148 ) ;
#5592 = EDGE_CURVE ( 'NONE', #43, #9873, #4204, .T. ) ;
#5593 = CLOSED_SHELL ( 'NONE', ( #3948, #11193, #11037, #2771, #1430, #9913, #7820, #5356, #7347, #9653, #3810, #11348, #4521, #11055, #5560, #9530, #8223, #4850, #8871, #3719, #7038, #4346, #6935, #10540, #3530, #7844, #10521, #5964, #9227, #11131, #8209, #11419, #10473, #570, #175, #11778, #4553, #9575, #4177, #11455, #7035, #1989, #3431, #3640, #8081, #6244, #3964, #5004, #1446, #3672, #6815, #1333, #710, #273, #8144, #1784, #7382, #10025, #6301, #10382, #10902, #1515, #9303, #2581, #11729, #4418, #558, #8887 ) ) ;
#5594 = CARTESIAN_POINT ( 'NONE',  ( -79.15625000000000000, 44.64466094067262958, 25.00000000000001066 ) ) ;
#5595 = B_SPLINE_CURVE_WITH_KNOTS ( 'NONE', 3,
 ( #4596, #6351, #868, #11772, #8195, #5386, #8134, #6233 ),
 .UNSPECIFIED., .F., .F.,
 ( 4, 2, 2, 4 ),
 ( 0.002921158011986725936, 0.003648658599403077456, 0.004376159186819428108, 0.005831160361652132015 ),
 .UNSPECIFIED. ) ;
#5596 = CARTESIAN_POINT ( 'NONE',  ( -72.96875000204838102, 80.81189881250000440, -1.580522963032174394E-15 ) ) ;
#5597 = LINE ( 'NONE', #11081, #393 ) ;
#5598 = FACE_BOUND ( 'NONE', #4430, .T. ) ;
#5599 = CARTESIAN_POINT ( 'NONE',  ( -65.75702278283388580, 54.97107188852366733, 0.01144463408162874063 ) ) ;
#5600 = SHAPE_DEFINITION_REPRESENTATION ( #5591, #6185 ) ;
#5601 = CARTESIAN_POINT ( 'NONE',  ( -7.621884045487905546, 66.99230996961183848, -18.44821524278371427 ) ) ;
#5602 = DIRECTION ( 'NONE',  ( 0.000000000000000000, 0.000000000000000000, 1.000000000000000000 ) ) ;
#5603 = ORIENTED_EDGE ( 'NONE', *, *, #6691, .F. ) ;
#5604 = DIRECTION ( 'NONE',  ( 1.000000000000000000, 6.033820786006286457E-17, -0.000000000000000000 ) ) ;
#5605 = LINE ( 'NONE', #11208, #766 ) ;
#5606 = ORIENTED_EDGE ( 'NONE', *, *, #2033, .T. ) ;
#5607 = CARTESIAN_POINT ( 'NONE',  ( 6.058385820703728442, 34.79737119409461599, 6.139092558150637480 ) ) ;
#5608 = CARTESIAN_POINT ( 'NONE',  ( -71.65625000204838102, 80.81189881250000440, -1.580522963032174394E-15 ) ) ;
#5609 = LINE ( 'NONE', #9248, #11493 ) ;
#5610 = CARTESIAN_POINT ( 'NONE',  ( -13.85565285731654761, 75.43037139504293975, 5.490367781071763709 ) ) ;
#5611 =( LENGTH_UNIT ( ) NAMED_UNIT ( * ) SI_UNIT ( .MILLI., .METRE. ) );
#5612 = CARTESIAN_POINT ( 'NONE',  ( -52.00383529082647271, 74.42722782460430153, 8.047526119559261559 ) ) ;
#5613 = EDGE_LOOP ( 'NONE', ( #3304, #128 ) ) ;
#5614 = DIRECTION ( 'NONE',  ( 0.000000000000000000, 0.000000000000000000, 1.000000000000000000 ) ) ;
#5615 = CARTESIAN_POINT ( 'NONE',  ( 3.571755578639977724, 50.00000000000001421, 2.874253840576960811E-12 ) ) ;
#5616 = CARTESIAN_POINT ( 'NONE',  ( -78.31250000000004263, 72.67766952966363192, -17.67766952966363903 ) ) ;
#5617 = ORIENTED_EDGE ( 'NONE', *, *, #11056, .T. ) ;
#5618 = CARTESIAN_POINT ( 'NONE',  ( -21.17314274085600090, 59.12512438474372090, 20.69754144995899026 ) ) ;
#5619 = CARTESIAN_POINT ( 'NONE',  ( -59.27472368810988002, 61.13901599248961105, 20.20251803659174783 ) ) ;
#5620 = CARTESIAN_POINT ( 'NONE',  ( 2.500000000000005773, 4.330127018922190985, -6.099999999999999645 ) ) ;
#5621 = DIRECTION ( 'NONE',  ( -1.000000000000000000, -0.000000000000000000, -0.000000000000000000 ) ) ;
#5622 = DIRECTION ( 'NONE',  ( 0.000000000000000000, 0.000000000000000000, 1.000000000000000000 ) ) ;
#5623 = LINE ( 'NONE', #3256, #10905 ) ;
#5624 = ORIENTED_EDGE ( 'NONE', *, *, #1294, .T. ) ;
#5625 = LINE ( 'NONE', #90, #590 ) ;
#5626 = CARTESIAN_POINT ( 'NONE',  ( -18.83686826543840453, 54.99741186838863882, -0.002939892491207554172 ) ) ;
#5627 = CARTESIAN_POINT ( 'NONE',  ( -49.68512622689396352, 59.96742314939218943, 0.6560827949113757773 ) ) ;
#5628 = CARTESIAN_POINT ( 'NONE',  ( 0.000000000000000000, -57.00000000000000000, 0.000000000000000000 ) ) ;
#5629 = CARTESIAN_POINT ( 'NONE',  ( 19.99999999999996803, -57.00000000000000000, -5.000000000000000000 ) ) ;
#5630 = CARTESIAN_POINT ( 'NONE',  ( -62.21092016019122894, 52.94303745291883700, 13.86761892224957116 ) ) ;
#5631 = ORIENTED_EDGE ( 'NONE', *, *, #6188, .F. ) ;
#5632 = CARTESIAN_POINT ( 'NONE',  ( 0.000000000000000000, 0.000000000000000000, -6.099999999999999645 ) ) ;
#5633 = UNCERTAINTY_MEASURE_WITH_UNIT (LENGTH_MEASURE( 1.000000000000000082E-05 ), #3108, 'distance_accuracy_value', 'NONE');
#5634 = VECTOR ( 'NONE', #8505, 1000.000000000000000 ) ;
#5635 = CARTESIAN_POINT ( 'NONE',  ( -80.00000000000002842, 46.51471862576140381, 3.371917798797308130E-06 ) ) ;
#5636 = DIRECTION ( 'NONE',  ( 0.000000000000000000, 0.000000000000000000, 1.000000000000000000 ) ) ;
#5637 = DIRECTION ( 'NONE',  ( 0.000000000000000000, -1.000000000000000000, 0.000000000000000000 ) ) ;
#5638 = CARTESIAN_POINT ( 'NONE',  ( -71.59560441993426139, 80.81189881250000440, 6.916273537586018705 ) ) ;
#5639 = CARTESIAN_POINT ( 'NONE',  ( -76.90625000204839523, 36.74823131438026280, 18.25176868561974786 ) ) ;
#5640 = ORIENTED_EDGE ( 'NONE', *, *, #2572, .T. ) ;
#5641 = VERTEX_POINT ( 'NONE', #8137 ) ;
#5642 = DIRECTION ( 'NONE',  ( -1.000000000000000000, -0.000000000000000000, -0.000000000000000000 ) ) ;
#5643 = CARTESIAN_POINT ( 'NONE',  ( -32.40470529452398551, 41.55719028461663100, -4.081861330394077392 ) ) ;
#5644 = CARTESIAN_POINT ( 'NONE',  ( -15.00000000000000000, -24.99999999999999645, -10.00000000000000000 ) ) ;
#5645 = CARTESIAN_POINT ( 'NONE',  ( -2.981862520314375153, 3.662834394221259390E-16, -0.01270000000000047133 ) ) ;
#5646 = CYLINDRICAL_SURFACE ( 'NONE', #6869, 1.499999999999999556 ) ;
#5647 = VERTEX_POINT ( 'NONE', #8981 ) ;
#5648 = CARTESIAN_POINT ( 'NONE',  ( -78.59375000000001421, 44.64466094067260826, -24.99999999999998934 ) ) ;
#5649 = CARTESIAN_POINT ( 'NONE',  ( -76.71875000409679046, 65.35533905932737753, 24.99999999999999645 ) ) ;
#5650 = FACE_OUTER_BOUND ( 'NONE', #2730, .T. ) ;
#5651 = CARTESIAN_POINT ( 'NONE',  ( -78.00000000000002842, 54.99999999999998579, 15.47056612039490986 ) ) ;
#5652 = EDGE_CURVE ( 'NONE', #9870, #7798, #2516, .T. ) ;
#5653 = CARTESIAN_POINT ( 'NONE',  ( -14.58248992847019920, 61.22172256553918146, 3.321057901781169885 ) ) ;
#5654 = APPLICATION_PROTOCOL_DEFINITION ( 'draft international standard', 'automotive_design', 1998, #7011 ) ;
#5655 = VECTOR ( 'NONE', #8671, 1000.000000000000000 ) ;
#5656 = CARTESIAN_POINT ( 'NONE',  ( -21.03106668926508149, 76.42784099770780415, 4.997211433137191960 ) ) ;
#5657 = CARTESIAN_POINT ( 'NONE',  ( 2.782474192756827142E-15, 65.42943686846950868, -22.72062601704910634 ) ) ;
#5658 = VERTEX_POINT ( 'NONE', #11600 ) ;
#5659 = DIRECTION ( 'NONE',  ( 0.000000000000000000, 0.000000000000000000, 1.000000000000000000 ) ) ;
#5660 = EDGE_CURVE ( 'NONE', #6052, #847, #10447, .T. ) ;
#5661 = DIRECTION ( 'NONE',  ( 1.000000000000000000, 0.000000000000000000, 0.000000000000000000 ) ) ;
#5662 = ADVANCED_FACE ( 'NONE', ( #11287 ), #2249, .F. ) ;
#5663 = ORIENTED_EDGE ( 'NONE', *, *, #10552, .F. ) ;
#5664 = CARTESIAN_POINT ( 'NONE',  ( -1.144262565995328940, 42.07883645215377300, -16.80394782698530065 ) ) ;
#5665 = CARTESIAN_POINT ( 'NONE',  ( -72.87500000204839523, 65.69163855873949842, 25.81189881250000440 ) ) ;
#5666 = CARTESIAN_POINT ( 'NONE',  ( -80.00000000000002842, 38.02943725152282184, 3.371917797929946392E-06 ) ) ;
#5667 = VECTOR ( 'NONE', #7834, 1000.000000000000114 ) ;
#5668 = DIRECTION ( 'NONE',  ( -1.000000000000000000, -0.000000000000000000, -0.000000000000000000 ) ) ;
#5669 = CARTESIAN_POINT ( 'NONE',  ( -2.188986190505546769, 52.25407376895000056, -20.97627476078892528 ) ) ;
#5670 = CARTESIAN_POINT ( 'NONE',  ( -34.14426257084027583, 36.62727174719971401, -10.58198811264723282 ) ) ;
#5671 = VERTEX_POINT ( 'NONE', #10507 ) ;
#5672 = PLANE ( 'NONE',  #8947 ) ;
#5673 = FACE_BOUND ( 'NONE', #7111, .T. ) ;
#5674 = CARTESIAN_POINT ( 'NONE',  ( 19.85574934264614910, 73.36821619702706698, 10.58005382006121131 ) ) ;
#5675 = VECTOR ( 'NONE', #11700, 1000.000000000000000 ) ;
#5676 = EDGE_LOOP ( 'NONE', ( #5932, #425, #6634, #683 ) ) ;
#5677 = CARTESIAN_POINT ( 'NONE',  ( -15.94161418140128994, 73.62867900310379810, 9.945362048789077036 ) ) ;
#5678 = CARTESIAN_POINT ( 'NONE',  ( 10.20626039314592681, 47.94399561767391305, 12.25029052866368673 ) ) ;
#5679 = CARTESIAN_POINT ( 'NONE',  ( -73.25000000409677625, 30.00000000000000355, 4.592425496802573578E-15 ) ) ;
#5680 = CARTESIAN_POINT ( 'NONE',  ( -78.12500000409677625, 55.00000000000000000, 24.99999999999999645 ) ) ;
#5681 = MECHANICAL_DESIGN_GEOMETRIC_PRESENTATION_REPRESENTATION (  '', ( #7397 ), #9110 ) ;
#5682 = CARTESIAN_POINT ( 'NONE',  ( 39.99999999999999289, 55.00000000000000000, 0.000000000000000000 ) ) ;
#5683 = CARTESIAN_POINT ( 'NONE',  ( -75.87500000409677625, 55.00000000000000000, -24.99999999999999645 ) ) ;
#5684 = EDGE_LOOP ( 'NONE', ( #7095, #10828, #11669, #5524 ) ) ;
#5685 = EDGE_CURVE ( 'NONE', #8040, #7395, #11837, .T. ) ;
#5686 = CARTESIAN_POINT ( 'NONE',  ( -19.71439386582751752, 54.99634062743773910, -0.004164711759880548002 ) ) ;
#5687 = CARTESIAN_POINT ( 'NONE',  ( -53.95632792247587162, 58.30500826365688738, 3.766154981294819404 ) ) ;
#5688 = DIRECTION ( 'NONE',  ( -0.8191520442889974607, 0.000000000000000000, -0.5735764363510379438 ) ) ;
#5689 = PRODUCT_DEFINITION_SHAPE ( 'NONE', 'NONE',  #11860 ) ;
#5690 = AXIS2_PLACEMENT_3D ( 'NONE', #11546, #8694, #6733 ) ;
#5691 = LINE ( 'NONE', #4724, #3772 ) ;
#5692 = CARTESIAN_POINT ( 'NONE',  ( 9.109914677241386372, 50.71033554483514649, 5.585537211039464545 ) ) ;
#5693 = CONICAL_SURFACE ( 'NONE', #10264, 2.500000000000000000, 0.9599310885968755924 ) ;
#5694 = ORIENTED_EDGE ( 'NONE', *, *, #2362, .F. ) ;
#5695 = CARTESIAN_POINT ( 'NONE',  ( 23.47754340821147068, 75.43020022661498558, 5.490793176664390707 ) ) ;
#5696 = DIRECTION ( 'NONE',  ( 1.000000000000000000, 6.033820786006286457E-17, -0.000000000000000000 ) ) ;
#5697 = CARTESIAN_POINT ( 'NONE',  ( -78.00000000000001421, 63.48528137423857487, -8.485278002320759683 ) ) ;
#5698 = LINE ( 'NONE', #100, #9310 ) ;
#5699 = CARTESIAN_POINT ( 'NONE',  ( -19.95440955002869288, 75.55706508317430803, -14.23123435947546511 ) ) ;
#5700 = CARTESIAN_POINT ( 'NONE',  ( -71.65625000204838102, 80.81189881250000440, -1.580522963032174394E-15 ) ) ;
#5701 = ORIENTED_EDGE ( 'NONE', *, *, #2033, .F. ) ;
#5702 = CIRCLE ( 'NONE', #6665, 4.999999999999984013 ) ;
#5703 = CARTESIAN_POINT ( 'NONE',  ( -72.68750000204839523, 65.69163855873949842, 25.81189881250000440 ) ) ;
#5704 = EDGE_LOOP ( 'NONE', ( #749, #411, #8667, #5915 ) ) ;
#5705 = CARTESIAN_POINT ( 'NONE',  ( 25.23800105611221767, 79.95549307754095025, 1.714966265850949689 ) ) ;
#5706 = CIRCLE ( 'NONE', #6472, 1.500000000000001332 ) ;
#5707 = CARTESIAN_POINT ( 'NONE',  ( -50.49690380378408605, 68.79103478457420806, 2.747024645387534214 ) ) ;
#5708 = EDGE_CURVE ( 'NONE', #1153, #3359, #2189, .T. ) ;
#5709 = LINE ( 'NONE', #6672, #8830 ) ;
#5710 = CARTESIAN_POINT ( 'NONE',  ( -75.00000000000008527, 62.52349484992671336, -24.64253936146262802 ) ) ;
#5711 = EDGE_CURVE ( 'NONE', #10129, #10562, #1356, .T. ) ;
#5712 = CARTESIAN_POINT ( 'NONE',  ( -80.00000000000000000, 55.00000000000000000, -20.00000000000000355 ) ) ;
#5713 = VERTEX_POINT ( 'NONE', #505 ) ;
#5714 = CARTESIAN_POINT ( 'NONE',  ( -78.50000000000000000, 55.00000000000000000, -24.99999999999999645 ) ) ;
#5715 = DIRECTION ( 'NONE',  ( 0.000000000000000000, 0.000000000000000000, 1.000000000000000000 ) ) ;
#5716 = CARTESIAN_POINT ( 'NONE',  ( 53.00000000000000000, 51.46446609406726935, 3.535533905932731091 ) ) ;
#5717 = FACE_BOUND ( 'NONE', #6170, .T. ) ;
#5718 = EDGE_CURVE ( 'NONE', #5990, #443, #3243, .T. ) ;
#5719 = B_SPLINE_CURVE_WITH_KNOTS ( 'NONE', 3,
 ( #1793, #11739, #9944, #7213, #3662, #3488, #9053, #829, #7378, #4502, #7153, #11005, #2817, #1678, #5519, #5460, #10776, #2762, #11796, #9108, #6485, #888, #6423, #8155, #2589, #3602, #7267, #10897, #6372, #10112, #8938, #716, #4563, #4387, #3121, #7506, #9343, #5705, #9404, #8392, #2156, #3775, #3957, #1132, #6729, #1198, #8457, #7619, #107, #235, #8573, #6609, #4921, #3899, #4673, #2880, #10361, #5827, #4862, #7676, #4799, #2030, #10236, #352, #8326, #7562, #8512, #7443, #11186, #2999, #9465, #6668, #171, #2093, #5766, #10180 ),
 .UNSPECIFIED., .F., .F.,
 ( 4, 2, 2, 2, 2, 2, 2, 2, 2, 2, 2, 2, 2, 2, 2, 2, 2, 2, 2, 2, 2, 2, 2, 2, 2, 2, 2, 2, 2, 2, 2, 2, 2, 2, 2, 2, 2, 4 ),
 ( 0.07733197755222971648, 0.07860774102649789596, 0.07988350450076606157, 0.08243503144930242055, 0.08371079492357058616, 0.08498655839783876564, 0.08753808534637511074, 0.09008961229491145584, 0.09264113924344780093, 0.09774419314052049113, 0.09901995661478867061, 0.1002957200890568501, 0.1028472470375931952, 0.1053987739861295403, 0.1066745374603977198, 0.1079503009346658993, 0.1130533548317386588, 0.1143291183060068522, 0.1156048817802750456, 0.1181564087288114462, 0.1194321722030796395, 0.1207079356773478329, 0.1232594626258842058, 0.1245352261001523991, 0.1258109895744205786, 0.1283625165229569931, 0.1309140434714933798, 0.1321898069457616010, 0.1334655704200297666, 0.1385686243171025123, 0.1411201512656388712, 0.1436716782141752302, 0.1487747321112479759, 0.1500504955855161415, 0.1513262590597843626, 0.1538777860083207216, 0.1564293129568570806, 0.1589808399053934673 ),
 .UNSPECIFIED. ) ;
#5720 = CARTESIAN_POINT ( 'NONE',  ( -67.32905043534587719, 54.99390458312336705, -0.002695445133683335107 ) ) ;
#5721 = VECTOR ( 'NONE', #5338, 1000.000000000000114 ) ;
#5722 = CARTESIAN_POINT ( 'NONE',  ( -12.86109194577659132, 70.12932790242416559, 15.98028952803886860 ) ) ;
#5723 = DIRECTION ( 'NONE',  ( 0.000000000000000000, -1.000000000000000000, 0.000000000000000000 ) ) ;
#5724 = ORIENTED_EDGE ( 'NONE', *, *, #10406, .F. ) ;
#5725 = PLANE ( 'NONE',  #1481 ) ;
#5726 = ADVANCED_FACE ( 'NONE', ( #3211 ), #9563, .F. ) ;
#5727 = CARTESIAN_POINT ( 'NONE',  ( -74.09375000409677625, 80.00000000000001421, -10.35533905932737753 ) ) ;
#5728 = ORIENTED_EDGE ( 'NONE', *, *, #4409, .T. ) ;
#5729 = CARTESIAN_POINT ( 'NONE',  ( -31.26269038945179446, 34.87416470039633509, 6.107602927758665423 ) ) ;
#5730 = CARTESIAN_POINT ( 'NONE',  ( 0.000000000000000000, 0.000000000000000000, -1.403639088038009630 ) ) ;
#5731 = CARTESIAN_POINT ( 'NONE',  ( -58.69833756168564065, 56.03204939003842355, 20.99267139547387373 ) ) ;
#5732 = PRESENTATION_STYLE_ASSIGNMENT (( #1347 ) ) ;
#5733 = CIRCLE ( 'NONE', #1120, 1.500000000000001332 ) ;
#5734 = CARTESIAN_POINT ( 'NONE',  ( -15.00000000000000000, -30.00000000000000000, 10.00000000000000000 ) ) ;
#5735 = ORIENTED_EDGE ( 'NONE', *, *, #2060, .F. ) ;
#5736 = CARTESIAN_POINT ( 'NONE',  ( -72.40625000204839523, 36.74823131438026280, 18.25176868561974786 ) ) ;
#5737 = CARTESIAN_POINT ( 'NONE',  ( 1.627231888947060723, 50.25466374745918330, -1.609084181729487639 ) ) ;
#5738 = CARTESIAN_POINT ( 'NONE',  ( 9.810937555461070048, 42.10554236623130464, 16.77741859935663626 ) ) ;
#5739 = ORIENTED_EDGE ( 'NONE', *, *, #996, .F. ) ;
#5740 = CARTESIAN_POINT ( 'NONE',  ( -39.82693389173066834, 50.89060194957639283, -20.69199581875299643 ) ) ;
#5741 = CARTESIAN_POINT ( 'NONE',  ( -50.85567158358731632, 75.98119253013058483, -2.745941642920928683 ) ) ;
#5742 = CARTESIAN_POINT ( 'NONE',  ( -5.000000000000000888, 0.000000000000000000, 0.000000000000000000 ) ) ;
#5743 = CARTESIAN_POINT ( 'NONE',  ( -78.00000000000002842, 42.27207793864211283, 4.242644059037075976 ) ) ;
#5744 = CIRCLE ( 'NONE', #1137, 1.500000000000001332 ) ;
#5745 = ADVANCED_FACE ( 'NONE', ( #9500 ), #269, .F. ) ;
#5746 = DIRECTION ( 'NONE',  ( 0.000000000000000000, 0.000000000000000000, 1.000000000000000000 ) ) ;
#5747 = CARTESIAN_POINT ( 'NONE',  ( -78.00000000000002842, 42.27207793864211283, 14.22792543327562775 ) ) ;
#5748 = ORIENTED_EDGE ( 'NONE', *, *, #8584, .F. ) ;
#5749 = CARTESIAN_POINT ( 'NONE',  ( -75.03125000000000000, 80.00000000000001421, 10.35533905932737397 ) ) ;
#5750 = CARTESIAN_POINT ( 'NONE',  ( -74.99999999999997158, 56.78048500034128665, -25.76437121692205423 ) ) ;
#5751 = DIRECTION ( 'NONE',  ( 0.000000000000000000, 1.000000000000000000, 0.000000000000000000 ) ) ;
#5752 = CARTESIAN_POINT ( 'NONE',  ( -74.37500000409677625, 55.00000000000000000, -24.99999999999999645 ) ) ;
#5753 = CIRCLE ( 'NONE', #566, 29.00000000000000355 ) ;
#5754 = CARTESIAN_POINT ( 'NONE',  ( 0.000000000000000000, 0.000000000000000000, -6.074599999999999334 ) ) ;
#5755 = CARTESIAN_POINT ( 'NONE',  ( 3.083722735221986255, 48.01900164405483196, -0.6869154824850737251 ) ) ;
#5756 = ORIENTED_EDGE ( 'NONE', *, *, #11547, .F. ) ;
#5757 = CARTESIAN_POINT ( 'NONE',  ( 4.003855478097921861, 35.57747403031575573, -8.044509115018048107 ) ) ;
#5758 = CARTESIAN_POINT ( 'NONE',  ( 0.000000000000000000, 0.000000000000000000, -3.832189483390572970 ) ) ;
#5759 = DIRECTION ( 'NONE',  ( 9.813077866773612233E-16, -1.000000000000000000, -0.000000000000000000 ) ) ;
#5760 = DIRECTION ( 'NONE',  ( -1.000000000000000000, -0.000000000000000000, -0.000000000000000000 ) ) ;
#5761 = CARTESIAN_POINT ( 'NONE',  ( -25.03138265018328568, 79.77837991132803097, -3.428720668973124663 ) ) ;
#5762 = CARTESIAN_POINT ( 'NONE',  ( -72.50000000204839523, 29.18810118750000981, 10.69163855873950020 ) ) ;
#5763 = ORIENTED_EDGE ( 'NONE', *, *, #11646, .F. ) ;
#5764 = CARTESIAN_POINT ( 'NONE',  ( -72.87500000204840944, 80.81189881250001861, 10.69163855873948599 ) ) ;
#5765 = FACE_BOUND ( 'NONE', #635, .T. ) ;
#5766 = CARTESIAN_POINT ( 'NONE',  ( 0.8611532375456804056, 65.42943686846948026, -22.72062601704910278 ) ) ;
#5767 = CARTESIAN_POINT ( 'NONE',  ( -60.40957880102118338, 50.93284021614062596, 13.40225281893947340 ) ) ;
#5768 = CIRCLE ( 'NONE', #1728, 3.000000000000000000 ) ;
#5769 = CARTESIAN_POINT ( 'NONE',  ( -78.68750000204838102, 44.30836144126052289, 25.81189881250000795 ) ) ;
#5770 = CARTESIAN_POINT ( 'NONE',  ( -78.00000000000001421, 67.72792206135787296, -2.742637315201482462 ) ) ;
#5771 = CIRCLE ( 'NONE', #2513, 5.000000000000000888 ) ;
#5772 = CARTESIAN_POINT ( 'NONE',  ( 53.00000000000000000, 47.00000000000000711, 6.000000000000000000 ) ) ;
#5773 = EDGE_LOOP ( 'NONE', ( #6687, #744, #5387, #11813 ) ) ;
#5774 = CIRCLE ( 'NONE', #6546, 4.999999999999997335 ) ;
#5775 = CIRCLE ( 'NONE', #7302, 2.500000000000000000 ) ;
#5776 = DIRECTION ( 'NONE',  ( 0.000000000000000000, 1.000000000000000000, 0.000000000000000000 ) ) ;
#5777 = CARTESIAN_POINT ( 'NONE',  ( -73.34375000409679046, 30.00000000000001421, 10.35533905932739174 ) ) ;
#5778 = CARTESIAN_POINT ( 'NONE',  ( -51.65302243398222970, 59.96738868206218598, -0.6562502162082396451 ) ) ;
#5779 = EDGE_LOOP ( 'NONE', ( #8863, #3238, #3032, #9369 ) ) ;
#5780 = EDGE_CURVE ( 'NONE', #7355, #10318, #5744, .T. ) ;
#5781 = CARTESIAN_POINT ( 'NONE',  ( -5.541508246797579140, 58.60498886477284941, -6.015263639686886599 ) ) ;
#5782 = CARTESIAN_POINT ( 'NONE',  ( -72.59375000000008527, 44.64466094067266511, -24.99999999999984723 ) ) ;
#5783 = EDGE_CURVE ( 'NONE', #818, #8222, #7766, .T. ) ;
#5784 = CIRCLE ( 'NONE', #3099, 1.500000000000001332 ) ;
#5785 = DIRECTION ( 'NONE',  ( 0.000000000000000000, 1.000000000000000000, 0.000000000000000000 ) ) ;
#5786 = VECTOR ( 'NONE', #4401, 1000.000000000000000 ) ;
#5787 = ORIENTED_EDGE ( 'NONE', *, *, #6186, .T. ) ;
#5788 = CARTESIAN_POINT ( 'NONE',  ( 36.99999999999999289, 55.00000000000000000, 0.000000000000000000 ) ) ;
#5789 = LINE ( 'NONE', #10968, #11091 ) ;
#5790 = EDGE_CURVE ( 'NONE', #6077, #5487, #8547, .T. ) ;
#5791 = ORIENTED_EDGE ( 'NONE', *, *, #4460, .T. ) ;
#5792 = CARTESIAN_POINT ( 'NONE',  ( -48.52239103406665066, 73.33336493528216238, -10.56581381373428208 ) ) ;
#5793 = APPLICATION_CONTEXT ( 'automotive_design' ) ;
#5794 = CARTESIAN_POINT ( 'NONE',  ( -73.15625000204839523, 73.25176868561975141, -18.25176868561974430 ) ) ;
#5795 = CARTESIAN_POINT ( 'NONE',  ( -2.500000000000000000, 3.061616997868383141E-16, -4.860324802323723326 ) ) ;
#5796 = CARTESIAN_POINT ( 'NONE',  ( -79.25000000000000000, 55.00000000000000000, 24.99999999999999645 ) ) ;
#5797 = CARTESIAN_POINT ( 'NONE',  ( -78.00000000000000000, 50.00000000000000000, 6.123233995736758394E-16 ) ) ;
#5798 = VERTEX_POINT ( 'NONE', #5024 ) ;
#5799 = CARTESIAN_POINT ( 'NONE',  ( -71.56250000204840944, 80.81189881250000440, -10.69163855873948954 ) ) ;
#5800 = CARTESIAN_POINT ( 'NONE',  ( -0.3234080915047974902, 51.02589827434706393, -3.051885828346310614 ) ) ;
#5801 = CARTESIAN_POINT ( 'NONE',  ( -78.40625000000005684, 65.35533905932518906, -25.00000000000207478 ) ) ;
#5802 = ORIENTED_EDGE ( 'NONE', *, *, #10537, .F. ) ;
#5803 = CARTESIAN_POINT ( 'NONE',  ( 8.144347139672229119, 36.66824632778702409, 10.56543010816455386 ) ) ;
#5804 = CARTESIAN_POINT ( 'NONE',  ( -45.83980951013849392, 66.71822699054862937, -17.55167914569291554 ) ) ;
#5805 = CARTESIAN_POINT ( 'NONE',  ( -78.78125000000002842, 30.00000000000003553, -10.35533905932737042 ) ) ;
#5806 = CARTESIAN_POINT ( 'NONE',  ( -80.00000000000002842, 50.75735931288069480, 4.242644059037076865 ) ) ;
#5807 = CARTESIAN_POINT ( 'NONE',  ( -80.00000000000001421, 63.48528137423857487, 6.985284746156351865 ) ) ;
#5808 = CARTESIAN_POINT ( 'NONE',  ( -75.12500000409677625, 55.00000000000000000, 24.99999999999999645 ) ) ;
#5809 = ORIENTED_EDGE ( 'NONE', *, *, #10689, .F. ) ;
#5810 = CARTESIAN_POINT ( 'NONE',  ( -74.75000000000000000, 55.00000000000000000, 24.99999999999999645 ) ) ;
#5811 = LINE ( 'NONE', #8619, #10807 ) ;
#5812 = ADVANCED_FACE ( 'NONE', ( #4957 ), #7828, .F. ) ;
#5813 = DIRECTION ( 'NONE',  ( -1.000000000000000000, -0.000000000000000000, -0.000000000000000000 ) ) ;
#5814 = DIRECTION ( 'NONE',  ( 0.000000000000000000, 0.000000000000000000, 1.000000000000000000 ) ) ;
#5815 = CARTESIAN_POINT ( 'NONE',  ( 14.55667984625315015, 56.83871188529325025, 6.833734452169164086 ) ) ;
#5816 = ORIENTED_EDGE ( 'NONE', *, *, #1242, .T. ) ;
#5817 = CARTESIAN_POINT ( 'NONE',  ( -42.07074724807011989, 61.10209548959944215, -20.11061483308460751 ) ) ;
#5818 = DIRECTION ( 'NONE',  ( -0.000000000000000000, -0.000000000000000000, -1.000000000000000000 ) ) ;
#5819 = FACE_OUTER_BOUND ( 'NONE', #5450, .T. ) ;
#5820 = EDGE_CURVE ( 'NONE', #6131, #7763, #5174, .T. ) ;
#5821 = LINE ( 'NONE', #9272, #1656 ) ;
#5822 = CARTESIAN_POINT ( 'NONE',  ( -25.29045292946807422, 80.00055243027901497, 0.3925393747600745553 ) ) ;
#5823 = CARTESIAN_POINT ( 'NONE',  ( -78.03125000204839523, 36.74823131438024859, -18.25176868561973720 ) ) ;
#5824 = ORIENTED_EDGE ( 'NONE', *, *, #7193, .T. ) ;
#5825 = CARTESIAN_POINT ( 'NONE',  ( -78.59375000409679046, 80.00000000000001421, -10.35533905932737753 ) ) ;
#5826 = CARTESIAN_POINT ( 'NONE',  ( -76.06250000000005684, 37.32233047033638940, 17.67766952966361771 ) ) ;
#5827 = CARTESIAN_POINT ( 'NONE',  ( 19.49008781870746176, 75.18049492239477161, -14.82407953042221038 ) ) ;
#5828 = CARTESIAN_POINT ( 'NONE',  ( -52.54481729858026995, 67.02647195319831042, 7.208015641604088586 ) ) ;
#5829 = CARTESIAN_POINT ( 'NONE',  ( -78.78125000204838102, 55.00000000000000000, 25.81189881249999729 ) ) ;
#5830 = DIRECTION ( 'NONE',  ( 1.000000000000000000, 0.000000000000000000, 0.000000000000000000 ) ) ;
#5831 = DIRECTION ( 'NONE',  ( -0.8660254037844380415, 0.5000000000000009992, 0.000000000000000000 ) ) ;
#5832 = ORIENTED_EDGE ( 'NONE', *, *, #8564, .F. ) ;
#5833 = CARTESIAN_POINT ( 'NONE',  ( -77.65625000000001421, 44.64466094067262958, 25.00000000000001066 ) ) ;
#5834 = CARTESIAN_POINT ( 'NONE',  ( -72.96875000409677625, 44.64466094067260826, -24.99999999999998934 ) ) ;
#5835 = CARTESIAN_POINT ( 'NONE',  ( -45.04238000299608302, 56.61143717230429928, -4.744501108842417381 ) ) ;
#5836 = ORIENTED_EDGE ( 'NONE', *, *, #2276, .T. ) ;
#5837 = CARTESIAN_POINT ( 'NONE',  ( -13.22334562740580921, 61.79442050427090294, 1.822429741926403501 ) ) ;
#5838 = CONTEXT_DEPENDENT_SHAPE_REPRESENTATION ( #2719, #5689 ) ;
#5839 = FACE_OUTER_BOUND ( 'NONE', #10994, .T. ) ;
#5840 = VERTEX_POINT ( 'NONE', #5918 ) ;
#5841 = CYLINDRICAL_SURFACE ( 'NONE', #8364, 4.999999999999984013 ) ;
#5842 = CARTESIAN_POINT ( 'NONE',  ( -76.71875000204839523, 36.74823131438024859, -18.25176868561973720 ) ) ;
#5843 = ORIENTED_EDGE ( 'NONE', *, *, #426, .F. ) ;
#5844 = CARTESIAN_POINT ( 'NONE',  ( -55.73751408985167899, 71.24607175163586703, 13.33484869932101269 ) ) ;
#5845 = CARTESIAN_POINT ( 'NONE',  ( -73.81250000204839523, 29.18810118750000981, 10.69163855873950020 ) ) ;
#5846 = B_SPLINE_CURVE_WITH_KNOTS ( 'NONE', 3,
 ( #11491, #11611, #8816, #10712, #9648, #7919, #1613, #8192 ),
 .UNSPECIFIED., .F., .F.,
 ( 4, 2, 2, 4 ),
 ( 0.002921158011986720298, 0.003648658599403072252, 0.004376159186819423771, 0.005831160361652126811 ),
 .UNSPECIFIED. ) ;
#5847 = PRESENTATION_LAYER_ASSIGNMENT (  '', '', ( #11169 ) ) ;
#5848 = CARTESIAN_POINT ( 'NONE',  ( -76.25000000000000000, 55.00000000000000000, 24.99999999999999645 ) ) ;
#5849 = DIRECTION ( 'NONE',  ( -1.000000000000000000, -0.000000000000000000, -0.000000000000000000 ) ) ;
#5850 =( LENGTH_UNIT ( ) NAMED_UNIT ( * ) SI_UNIT ( .MILLI., .METRE. ) );
#5851 = CARTESIAN_POINT ( 'NONE',  ( -78.03125000409679046, 44.64466094067260826, 24.99999999999998579 ) ) ;
#5852 = VERTEX_POINT ( 'NONE', #3035 ) ;
#5853 = CARTESIAN_POINT ( 'NONE',  ( -71.40810441781459872, 80.81189881250000440, 6.916273779317701376 ) ) ;
#5854 = DIRECTION ( 'NONE',  ( 0.000000000000000000, 0.000000000000000000, 1.000000000000000000 ) ) ;
#5855 = CARTESIAN_POINT ( 'NONE',  ( -33.30269350532120143, 33.99387206627966407, -1.031609878214063025 ) ) ;
#5856 = CONICAL_SURFACE ( 'NONE', #2395, 3.000000000000000888, 0.9599310885968804774 ) ;
#5857 = ORIENTED_EDGE ( 'NONE', *, *, #7203, .F. ) ;
#5858 = EDGE_CURVE ( 'NONE', #8444, #5404, #8372, .T. ) ;
#5859 = CARTESIAN_POINT ( 'NONE',  ( 23.66666666666668561, 76.00000000000000000, 0.000000000000000000 ) ) ;
#5860 = CARTESIAN_POINT ( 'NONE',  ( 18.79384863814433615, 66.18161908153624040, 8.591911950030317158 ) ) ;
#5861 = CARTESIAN_POINT ( 'NONE',  ( 14.99999999999999645, 55.00000000000000000, 20.00000000000000000 ) ) ;
#5862 = PLANE ( 'NONE',  #7194 ) ;
#5863 = DIRECTION ( 'NONE',  ( -0.8191520442889885789, 1.003171929053520802E-16, 0.5735764363510507113 ) ) ;
#5864 = EDGE_LOOP ( 'NONE', ( #2588, #3582, #8242, #5191 ) ) ;
#5865 =( BOUNDED_CURVE ( )  B_SPLINE_CURVE ( 2, ( #9872, #10766, #7144, #8988, #9214, #10224, #1961, #9153, #1899 ),
 .UNSPECIFIED., .F., .T. ) 
 B_SPLINE_CURVE_WITH_KNOTS ( ( 3, 2, 2, 2, 3 ),
 ( 0.000000000000000000, 0.02083333333333334952, 0.04166666666666669905, 0.06250000000000005551, 0.08333333333333339810 ),
 .UNSPECIFIED. ) 
 CURVE ( )  GEOMETRIC_REPRESENTATION_ITEM ( )  RATIONAL_B_SPLINE_CURVE ( ( 1.000000000000000000, 0.9238795325112867385, 1.000000000000000000, 0.9238795325112867385, 1.000000000000000000, 0.9238795325112867385, 1.000000000000000000, 0.9238795325112865164, 1.000000000000000222 ) ) 
 REPRESENTATION_ITEM ( '' )  );
#5866 = CARTESIAN_POINT ( 'NONE',  ( -79.25000000000000000, 55.00000000000000000, 24.99999999999999645 ) ) ;
#5867 = FACE_OUTER_BOUND ( 'NONE', #8315, .T. ) ;
#5868 = VECTOR ( 'NONE', #10519, 1000.000000000000000 ) ;
#5869 = CYLINDRICAL_SURFACE ( 'NONE', #1279, 24.99999999999999645 ) ;
#5870 = CARTESIAN_POINT ( 'NONE',  ( 13.77658176772798093, 55.91632091561838536, 6.982821974894761752 ) ) ;
#5871 = EDGE_LOOP ( 'NONE', ( #622, #666 ) ) ;
#5872 = CARTESIAN_POINT ( 'NONE',  ( -43.83980969374544401, 66.71858909844225138, -17.55257377017560216 ) ) ;
#5873 = VECTOR ( 'NONE', #2007, 1000.000000000000000 ) ;
#5874 = DIRECTION ( 'NONE',  ( 0.000000000000000000, 0.000000000000000000, 1.000000000000000000 ) ) ;
#5875 = EDGE_CURVE ( 'NONE', #9929, #9538, #4895, .T. ) ;
#5876 = CARTESIAN_POINT ( 'NONE',  ( -78.00000000000001421, 50.75735931288069480, -14.22791868944003646 ) ) ;
#5877 = CARTESIAN_POINT ( 'NONE',  ( -77.84375000204839523, 55.00000000000000000, -25.81189881249999729 ) ) ;
#5878 = CARTESIAN_POINT ( 'NONE',  ( -71.53052368722832455, 77.35376350879521112, 12.90594348738575903 ) ) ;
#5879 = ORIENTED_EDGE ( 'NONE', *, *, #11280, .T. ) ;
#5880 = CARTESIAN_POINT ( 'NONE',  ( -71.93750000204838102, 44.30836144126050158, -25.81189881249999374 ) ) ;
#5881 = FACE_BOUND ( 'NONE', #3929, .T. ) ;
#5882 = FILL_AREA_STYLE_COLOUR ( '', #10845 ) ;
#5883 = CARTESIAN_POINT ( 'NONE',  ( -29.78863982673286870, 41.14007247853228222, 2.056775689438067989 ) ) ;
#5884 = AXIS2_PLACEMENT_3D ( 'NONE', #7493, #4605, #2865 ) ;
#5885 = EDGE_CURVE ( 'NONE', #8444, #4583, #3328, .T. ) ;
#5886 = CARTESIAN_POINT ( 'NONE',  ( -80.00000000000000000, 55.00000000000000000, 0.000000000000000000 ) ) ;
#5887 = CARTESIAN_POINT ( 'NONE',  ( -15.00000000000000355, 5.000000000000000000, 30.00000000000000711 ) ) ;
#5888 = PLANE ( 'NONE',  #1683 ) ;
#5889 = ORIENTED_EDGE ( 'NONE', *, *, #7423, .F. ) ;
#5890 = CONICAL_SURFACE ( 'NONE', #9705, 3.000000000000000000, 0.9599310885968912466 ) ;
#5891 = CARTESIAN_POINT ( 'NONE',  ( -72.78125000000002842, 30.00000000000000355, -10.35533905932738108 ) ) ;
#5892 = CARTESIAN_POINT ( 'NONE',  ( -72.40625000409677625, 80.00000000000001421, 10.35533905932737397 ) ) ;
#5893 = CONICAL_SURFACE ( 'NONE', #10838, 3.000000000000000000, 0.9599310885968912466 ) ;
#5894 = ADVANCED_FACE ( 'NONE', ( #796 ), #4698, .F. ) ;
#5895 = CARTESIAN_POINT ( 'NONE',  ( -42.31849960451753390, 54.34441004806944875, -4.967488205851171124 ) ) ;
#5896 = ORIENTED_EDGE ( 'NONE', *, *, #11787, .T. ) ;
#5897 = CARTESIAN_POINT ( 'NONE',  ( 10.89008576165924680, 49.38437030094291913, 4.319752267554956227 ) ) ;
#5898 = DIRECTION ( 'NONE',  ( -1.000000000000000000, 0.000000000000000000, 0.000000000000000000 ) ) ;
#5899 = CARTESIAN_POINT ( 'NONE',  ( -80.00000000000001421, 63.48528137423857487, 8.485284746156350977 ) ) ;
#5900 = EDGE_LOOP ( 'NONE', ( #9837, #2204, #3455, #8371 ) ) ;
#5901 = CARTESIAN_POINT ( 'NONE',  ( 15.84255450020419964, 72.28565062628483417, -13.62130773388284055 ) ) ;
#5902 = CARTESIAN_POINT ( 'NONE',  ( -76.53125000204838102, 55.00000000000000000, -25.81189881249999729 ) ) ;
#5903 = ORIENTED_EDGE ( 'NONE', *, *, #2212, .F. ) ;
#5904 = CARTESIAN_POINT ( 'NONE',  ( -38.47762819156672265, 42.07891330237754346, -16.80402559754432801 ) ) ;
#5905 = DIRECTION ( 'NONE',  ( 6.033820786006286457E-17, -1.000000000000000000, 0.000000000000000000 ) ) ;
#5906 = VECTOR ( 'NONE', #2523, 1000.000000000000000 ) ;
#5907 = CARTESIAN_POINT ( 'NONE',  ( -75.31250000409677625, 72.67766952966368876, 17.67766952966368521 ) ) ;
#5908 = CARTESIAN_POINT ( 'NONE',  ( 0.000000000000000000, -30.00000000000000000, -5.000000000000000000 ) ) ;
#5909 = FILL_AREA_STYLE_COLOUR ( '', #81 ) ;
#5910 = CARTESIAN_POINT ( 'NONE',  ( 14.99999999999999645, 5.000000000000000000, -19.99999999999999645 ) ) ;
#5911 = ORIENTED_EDGE ( 'NONE', *, *, #10075, .F. ) ;
#5912 = CARTESIAN_POINT ( 'NONE',  ( 53.00000000000000000, 55.00000000000000000, 6.000000000000000000 ) ) ;
#5913 = PLANE ( 'NONE',  #5931 ) ;
#5914 = CARTESIAN_POINT ( 'NONE',  ( -36.85572911278101316, 38.22258139949027367, -12.89445763391127464 ) ) ;
#5915 = ORIENTED_EDGE ( 'NONE', *, *, #1152, .T. ) ;
#5916 = CARTESIAN_POINT ( 'NONE',  ( -16.60828084699550544, 73.62754440388609112, 9.944891948484055888 ) ) ;
#5917 = CARTESIAN_POINT ( 'NONE',  ( -9.998140069271334696, 64.90968168482568501, -9.910269716092365400 ) ) ;
#5918 = CARTESIAN_POINT ( 'NONE',  ( -2.500000000000000000, 3.061616997868383141E-16, -5.724496230895143256 ) ) ;
#5919 = CARTESIAN_POINT ( 'NONE',  ( -76.53125000409679046, 44.64466094067255142, 24.99999999999992184 ) ) ;
#5920 = UNCERTAINTY_MEASURE_WITH_UNIT (LENGTH_MEASURE( 1.000000000000000082E-05 ), #6512, 'distance_accuracy_value', 'NONE');
#5921 = UNCERTAINTY_MEASURE_WITH_UNIT (LENGTH_MEASURE( 1.000000000000000082E-05 ), #5850, 'distance_accuracy_value', 'NONE');
#5922 = DIRECTION ( 'NONE',  ( 1.000000000000000000, 6.033820786006286457E-17, -0.000000000000000000 ) ) ;
#5923 = AXIS2_PLACEMENT_3D ( 'NONE', #2677, #1591, #7298 ) ;
#5924 = ORIENTED_EDGE ( 'NONE', *, *, #1092, .F. ) ;
#5925 = CARTESIAN_POINT ( 'NONE',  ( -76.71875000204839523, 36.74823131438024859, -18.25176868561973720 ) ) ;
#5926 = CARTESIAN_POINT ( 'NONE',  ( -20.00000000000003197, -57.00000000000000000, -5.000000000000000000 ) ) ;
#5927 = CARTESIAN_POINT ( 'NONE',  ( 47.00000000000000000, 55.00000000000000000, 0.000000000000000000 ) ) ;
#5928 = CONICAL_SURFACE ( 'NONE', #1325, 2.450000000000000178, 0.9599310885968801443 ) ;
#5929 = CARTESIAN_POINT ( 'NONE',  ( 47.00000000000000000, 51.46446609406726935, -3.535533905932738197 ) ) ;
#5930 = CARTESIAN_POINT ( 'NONE',  ( -44.45858743606044072, 56.70130388464480831, -6.794919630703683211 ) ) ;
#5931 = AXIS2_PLACEMENT_3D ( 'NONE', #1570, #6816, #6761 ) ;
#5932 = ORIENTED_EDGE ( 'NONE', *, *, #2774, .F. ) ;
#5933 = CARTESIAN_POINT ( 'NONE',  ( -18.45202553953894764, 65.80723110900194683, 18.02933743899848551 ) ) ;
#5934 = DIRECTION ( 'NONE',  ( -1.000000000000000000, -0.000000000000000000, -0.000000000000000000 ) ) ;
#5935 = CYLINDRICAL_SURFACE ( 'NONE', #10778, 22.00000000000000000 ) ;
#5936 = EDGE_CURVE ( 'NONE', #7726, #10425, #11332, .T. ) ;
#5937 = CARTESIAN_POINT ( 'NONE',  ( -77.18750000204839523, 65.69163855873949842, 25.81189881250000084 ) ) ;
#5938 =( BOUNDED_SURFACE ( )  B_SPLINE_SURFACE ( 1, 2, ( 
 ( #9049, #6543, #8150, #11735, #5514, #9103, #7207, #42, #11790, #1736, #7373, #6306, #11000, #7263, #9161, #9994, #10892, #10832, #2876, #5401, #2639, #3535, #4612, #2702, #1789, #6368, #4558, #8268, #8208, #10948, #945, #6480, #11844, #1009, #10173, #2758, #8099, #6418, #11065, #10048, #5342, #1846, #3710, #2812, #3770, #10107, #5575, #9221, #4669, #8994, #769, #4446, #9520, #166, #4014, #4916, #3117, #9399, #3837, #2152, #2936, #7732, #1127, #11307, #11125, #11363, #8629, #1067, #4795, #2210, #10294, #10232, #1311, #3895, #4733, #5762, #9460, #9338, #8451, #10412, #2026, #7672, #3952, #6605, #5700, #231, #5878 ),
 ( #7557, #4977, #1194, #410, #11180, #2994, #8387, #7614, #7501, #9274, #6661, #4075, #2088, #3054, #5823, #288, #4858, #8508, #1969, #11243, #3172, #6724, #10355, #1246, #8568, #6840, #5639, #347, #6783, #525, #11417, #10635, #6059, #2383, #3288, #6957, #10524, #2332, #11659, #9636, #5039, #2448, #9694, #468, #5212, #1432, #6896, #641, #3228, #4303, #5095, #6114, #10583, #8742, #4125, #8021, #6003, #7788, #8686, #9748, #4186, #1491, #7848, #11476, #1545, #5151, #582, #8862, #11596, #8803, #6176, #3469, #4249, #1376, #7908, #4369, #11537, #10466, #3341, #7012, #7961, #8915, #3402, #7075, #10700, #2512, #9806 ) ),
 .UNSPECIFIED., .F., .F., .T. ) 
 B_SPLINE_SURFACE_WITH_KNOTS ( ( 2, 2 ),
 ( 3, 2, 2, 2, 2, 2, 2, 2, 2, 2, 2, 2, 2, 2, 2, 2, 2, 2, 2, 2, 2, 2, 2, 2, 2, 2, 2, 2, 2, 2, 2, 2, 2, 2, 2, 2, 2, 2, 2, 2, 2, 2, 2, 3 ),
 ( 0.000000000000000000, 1.000000000000000000 ),
 ( 0.000000000000000000, 0.02083333333333333218, 0.04166666666666666435, 0.06250000000000000000, 0.08333333333333332871, 0.1041666666666666713, 0.1250000000000000000, 0.1458333333333333426, 0.1666666666666666574, 0.1875000000000000000, 0.2083333333333333426, 0.2291666666666666574, 0.2500000000000000000, 0.2708333333333333148, 0.2916666666666666852, 0.3125000000000000000, 0.3333333333333333148, 0.3541666666666666852, 0.3750000000000000000, 0.3958333333333333148, 0.4166666666666666852, 0.4375000000000000000, 0.4583333333333333148, 0.4791666666666666852, 0.5000000000000000000, 0.5208333333333333703, 0.5416666666666666297, 0.5625000000000000000, 0.5833333333333333703, 0.6041666666666666297, 0.6250000000000000000, 0.6458333333333333703, 0.6666666666666666297, 0.6875000000000000000, 0.7083333333333333703, 0.7291666666666666297, 0.7500000000000000000, 0.7708333333333333703, 0.7916666666666666297, 0.8125000000000000000, 0.8333333333333333703, 0.8541666666666666297, 0.8750000000000000000, 0.8888490476107191451 ),
 .UNSPECIFIED. ) 
 GEOMETRIC_REPRESENTATION_ITEM ( )  RATIONAL_B_SPLINE_SURFACE ( (
 ( 1.000000000000000000, 0.9238795325112867385, 1.000000000000000000, 0.9238795325112867385, 1.000000000000000000, 0.9238795325112867385, 1.000000000000000000, 0.9238795325112867385, 1.000000000000000000, 0.9238795325112867385, 1.000000000000000000, 0.9238795325112867385, 1.000000000000000000, 0.9238795325112867385, 1.000000000000000000, 0.9238795325112867385, 1.000000000000000000, 0.9238795325112867385, 1.000000000000000000, 0.9238795325112867385, 1.000000000000000000, 0.9238795325112867385, 1.000000000000000000, 0.9238795325112867385, 1.000000000000000000, 0.9238795325112867385, 1.000000000000000000, 0.9238795325112867385, 1.000000000000000000, 0.9238795325112867385, 1.000000000000000000, 0.9238795325112867385, 1.000000000000000000, 0.9238795325112867385, 1.000000000000000000, 0.9238795325112867385, 1.000000000000000000, 0.9238795325112867385, 1.000000000000000000, 0.9238795325112867385, 1.000000000000000000, 0.9238795325112867385, 1.000000000000000000, 0.9238795325112867385, 1.000000000000000000, 0.9238795325112867385, 1.000000000000000000, 0.9238795325112867385, 1.000000000000000000, 0.9238795325112867385, 1.000000000000000000, 0.9238795325112867385, 1.000000000000000000, 0.9238795325112867385, 1.000000000000000000, 0.9238795325112867385, 1.000000000000000000, 0.9238795325112867385, 1.000000000000000000, 0.9238795325112867385, 1.000000000000000000, 0.9238795325112867385, 1.000000000000000000, 0.9238795325112867385, 1.000000000000000000, 0.9238795325112867385, 1.000000000000000000, 0.9238795325112867385, 1.000000000000000000, 0.9238795325112867385, 1.000000000000000000, 0.9238795325112867385, 1.000000000000000000, 0.9238795325112867385, 1.000000000000000000, 0.9238795325112867385, 1.000000000000000000, 0.9238795325112867385, 1.000000000000000000, 0.9238795325112867385, 1.000000000000000000, 0.9238795325112867385, 1.000000000000000000, 0.9238795325112867385, 1.000000000000000000, 0.9493985930367334625, 0.9660721903170175207),
 ( 1.000000000000000000, 0.9238795325112867385, 1.000000000000000000, 0.9238795325112867385, 1.000000000000000000, 0.9238795325112867385, 1.000000000000000000, 0.9238795325112867385, 1.000000000000000000, 0.9238795325112867385, 1.000000000000000000, 0.9238795325112867385, 1.000000000000000000, 0.9238795325112867385, 1.000000000000000000, 0.9238795325112867385, 1.000000000000000000, 0.9238795325112867385, 1.000000000000000000, 0.9238795325112867385, 1.000000000000000000, 0.9238795325112867385, 1.000000000000000000, 0.9238795325112867385, 1.000000000000000000, 0.9238795325112867385, 1.000000000000000000, 0.9238795325112867385, 1.000000000000000000, 0.9238795325112867385, 1.000000000000000000, 0.9238795325112867385, 1.000000000000000000, 0.9238795325112867385, 1.000000000000000000, 0.9238795325112867385, 1.000000000000000000, 0.9238795325112867385, 1.000000000000000000, 0.9238795325112867385, 1.000000000000000000, 0.9238795325112867385, 1.000000000000000000, 0.9238795325112867385, 1.000000000000000000, 0.9238795325112867385, 1.000000000000000000, 0.9238795325112867385, 1.000000000000000000, 0.9238795325112867385, 1.000000000000000000, 0.9238795325112867385, 1.000000000000000000, 0.9238795325112867385, 1.000000000000000000, 0.9238795325112867385, 1.000000000000000000, 0.9238795325112867385, 1.000000000000000000, 0.9238795325112867385, 1.000000000000000000, 0.9238795325112867385, 1.000000000000000000, 0.9238795325112867385, 1.000000000000000000, 0.9238795325112867385, 1.000000000000000000, 0.9238795325112867385, 1.000000000000000000, 0.9238795325112867385, 1.000000000000000000, 0.9238795325112867385, 1.000000000000000000, 0.9238795325112867385, 1.000000000000000000, 0.9238795325112867385, 1.000000000000000000, 0.9238795325112867385, 1.000000000000000000, 0.9238795325112867385, 1.000000000000000000, 0.9238795325112867385, 1.000000000000000000, 0.9238795325112867385, 1.000000000000000000, 0.9493985930367334625, 0.9660721903170175207) ) ) 
 REPRESENTATION_ITEM ( '' )  SURFACE ( )  );
#5939 = DIRECTION ( 'NONE',  ( 0.000000000000000000, 1.000000000000000000, 0.000000000000000000 ) ) ;
#5940 = CARTESIAN_POINT ( 'NONE',  ( 36.99999999999999289, 59.99999999999998579, 0.000000000000000000 ) ) ;
#5941 = EDGE_LOOP ( 'NONE', ( #2530, #1841, #5292, #252 ) ) ;
#5942 = CARTESIAN_POINT ( 'NONE',  ( -78.40625000409677625, 80.00000000000001421, 10.35533905932737397 ) ) ;
#5943 = DIRECTION ( 'NONE',  ( -1.000000000000000000, 0.000000000000000000, 0.000000000000000000 ) ) ;
#5944 = CONICAL_SURFACE ( 'NONE', #9561, 2.500000000000000000, 0.9599310885968755924 ) ;
#5945 = CARTESIAN_POINT ( 'NONE',  ( -75.87500000000007105, 30.00000000000010303, 4.592425496802555434E-15 ) ) ;
#5946 =( NAMED_UNIT ( * ) SI_UNIT ( $, .STERADIAN. ) SOLID_ANGLE_UNIT ( ) );
#5947 = CIRCLE ( 'NONE', #9565, 5.000000000000000888 ) ;
#5948 = CARTESIAN_POINT ( 'NONE',  ( -4.160267277967630406, 59.12176995062825569, -20.68921489609442332 ) ) ;
#5949 = FACE_OUTER_BOUND ( 'NONE', #1859, .T. ) ;
#5950 =( REPRESENTATION_RELATIONSHIP ('NONE','NONE', #5489, #6185 ) REPRESENTATION_RELATIONSHIP_WITH_TRANSFORMATION ( #1986 )SHAPE_REPRESENTATION_RELATIONSHIP( ) );
#5951 = CARTESIAN_POINT ( 'NONE',  ( 0.000000000000000000, 0.000000000000000000, -3.482085714285714229 ) ) ;
#5952 = CARTESIAN_POINT ( 'NONE',  ( 62.44550000000000267, 55.00000000000000000, -2.999999999999995559 ) ) ;
#5953 = EDGE_CURVE ( 'NONE', #678, #3881, #10493, .T. ) ;
#5954 = ORIENTED_EDGE ( 'NONE', *, *, #149, .T. ) ;
#5955 = CARTESIAN_POINT ( 'NONE',  ( -78.00000000000002842, 50.75735931288069480, 12.72792543327563131 ) ) ;
#5956 = EDGE_CURVE ( 'NONE', #5423, #1264, #3141, .T. ) ;
#5957 = ADVANCED_FACE ( 'NONE', ( #1401 ), #1411, .T. ) ;
#5958 = CARTESIAN_POINT ( 'NONE',  ( -77.18750000000000000, 37.32233047033631124, -17.67766952966368166 ) ) ;
#5959 = CARTESIAN_POINT ( 'NONE',  ( 37.00000000000000000, 60.00000000000000000, 6.123233995736769241E-16 ) ) ;
#5960 = CARTESIAN_POINT ( 'NONE',  ( 9.999999999999994671, -24.99999999999999645, 10.00000000000000000 ) ) ;
#5961 = ORIENTED_EDGE ( 'NONE', *, *, #10757, .T. ) ;
#5962 = CARTESIAN_POINT ( 'NONE',  ( -32.08425350687716104, 48.28742629341236636, -2.036605179622332784 ) ) ;
#5963 = AXIS2_PLACEMENT_3D ( 'NONE', #4554, #1843, #10104 ) ;
#5964 = ADVANCED_FACE ( 'NONE', ( #243 ), #7627, .F. ) ;
#5965 = EDGE_CURVE ( 'NONE', #7521, #10082, #5753, .T. ) ;
#5966 = DIRECTION ( 'NONE',  ( -0.000000000000000000, 0.000000000000000000, -1.000000000000000000 ) ) ;
#5967 = CARTESIAN_POINT ( 'NONE',  ( -80.00000000000001421, 50.75735931288069480, -4.242637315201482906 ) ) ;
#5968 = EDGE_CURVE ( 'NONE', #1776, #10196, #7685, .T. ) ;
#5969 = ORIENTED_EDGE ( 'NONE', *, *, #10336, .F. ) ;
#5970 = CARTESIAN_POINT ( 'NONE',  ( 20.05122251396076649, 75.61688920795575086, 7.685058149121978488 ) ) ;
#5971 = CIRCLE ( 'NONE', #772, 5.000000000000000000 ) ;
#5972 = CARTESIAN_POINT ( 'NONE',  ( -77.37500000204838102, 65.69163855873949842, 25.81189881250000084 ) ) ;
#5973 = EDGE_LOOP ( 'NONE', ( #6509, #862, #10132, #3846 ) ) ;
#5974 = CARTESIAN_POINT ( 'NONE',  ( -74.65625000204839523, 73.25176868561975141, -18.25176868561974430 ) ) ;
#5975 = FACE_OUTER_BOUND ( 'NONE', #6897, .T. ) ;
#5976 = CARTESIAN_POINT ( 'NONE',  ( 0.000000000000000000, 0.000000000000000000, -6.099999999999999645 ) ) ;
#5977 = CONICAL_SURFACE ( 'NONE', #9021, 2.500000000000000000, 0.9599310885968755924 ) ;
#5978 = CIRCLE ( 'NONE', #11298, 1.500000000000001332 ) ;
#5979 =( NAMED_UNIT ( * ) SI_UNIT ( $, .STERADIAN. ) SOLID_ANGLE_UNIT ( ) );
#5980 = DIRECTION ( 'NONE',  ( -6.033820786006286457E-17, 1.000000000000000000, 0.000000000000000000 ) ) ;
#5981 = ORIENTED_EDGE ( 'NONE', *, *, #11024, .F. ) ;
#5982 = DIRECTION ( 'NONE',  ( -1.000000000000000000, -0.000000000000000000, -0.000000000000000000 ) ) ;
#5983 = CARTESIAN_POINT ( 'NONE',  ( -29.49360042904642043, 37.45509264529403737, 11.71531283165970727 ) ) ;
#5984 = ORIENTED_EDGE ( 'NONE', *, *, #9211, .T. ) ;
#5985 = CARTESIAN_POINT ( 'NONE',  ( -5.493600489990522640, 59.12202052924457973, -20.68980504072543170 ) ) ;
#5986 = CARTESIAN_POINT ( 'NONE',  ( -21.96365303252882839, 59.72418919812645299, 13.20300428545286131 ) ) ;
#5987 = CIRCLE ( 'NONE', #5023, 1.500000000000001332 ) ;
#5988 = DIRECTION ( 'NONE',  ( -0.000000000000000000, 1.000000000000000000, 0.000000000000000000 ) ) ;
#5989 = CARTESIAN_POINT ( 'NONE',  ( 2.500000000000000000, 0.000000000000000000, -5.724496230895143256 ) ) ;
#5990 = VERTEX_POINT ( 'NONE', #5959 ) ;
#5991 = CARTESIAN_POINT ( 'NONE',  ( -72.96875000000000000, 30.00000000000001421, 10.35533905932739174 ) ) ;
#5992 = CYLINDRICAL_SURFACE ( 'NONE', #4130, 1.499999999999999556 ) ;
#5993 = CARTESIAN_POINT ( 'NONE',  ( -2.500000000000000000, 3.061616997868383141E-16, -3.996153373752295401 ) ) ;
#5994 = DIRECTION ( 'NONE',  ( 0.8191520442889974607, 1.003171929053531649E-16, -0.5735764363510379438 ) ) ;
#5995 = CARTESIAN_POINT ( 'NONE',  ( -23.75092017888364282, 55.68721295373460833, 6.987118555467080938 ) ) ;
#5996 = VERTEX_POINT ( 'NONE', #9596 ) ;
#5997 = CARTESIAN_POINT ( 'NONE',  ( -32.72515708217407138, 34.82695427582095959, -6.127117481167428714 ) ) ;
#5998 = CARTESIAN_POINT ( 'NONE',  ( 16.81101720596863203, 65.56606704192360269, 18.33326034385300574 ) ) ;
#5999 = DIRECTION ( 'NONE',  ( -1.000000000000000000, -0.000000000000000000, -0.000000000000000000 ) ) ;
#6000 = CARTESIAN_POINT ( 'NONE',  ( -78.40625000204839523, 36.74823131438026280, 18.25176868561974786 ) ) ;
#6001 = ADVANCED_FACE ( 'NONE', ( #5052 ), #183, .F. ) ;
#6002 = CARTESIAN_POINT ( 'NONE',  ( -0.8575857771174034694, 65.42943686846950868, 22.72062601704910634 ) ) ;
#6003 = CARTESIAN_POINT ( 'NONE',  ( -74.09375000204839523, 55.00000000000000000, 25.81189881249999729 ) ) ;
#6004 = VERTEX_POINT ( 'NONE', #3008 ) ;
#6005 = CARTESIAN_POINT ( 'NONE',  ( -72.31250000409677625, 72.67766952966368876, 17.67766952966368521 ) ) ;
#6006 = DIRECTION ( 'NONE',  ( 0.000000000000000000, 0.000000000000000000, 1.000000000000000000 ) ) ;
#6007 = LINE ( 'NONE', #6846, #5394 ) ;
#6008 = CARTESIAN_POINT ( 'NONE',  ( 5.737308841168996310, 34.06700459503902323, -2.059191599423306318 ) ) ;
#6009 = DIRECTION ( 'NONE',  ( 0.000000000000000000, 0.000000000000000000, 1.000000000000000000 ) ) ;
#6010 = DIRECTION ( 'NONE',  ( -1.000000000000000000, -0.000000000000000000, -0.000000000000000000 ) ) ;
#6011 =( BOUNDED_CURVE ( )  B_SPLINE_CURVE ( 2, ( #897, #3609, #7829, #8723, #11805, #5412, #8110, #6942, #7276 ),
 .UNSPECIFIED., .F., .T. ) 
 B_SPLINE_CURVE_WITH_KNOTS ( ( 3, 2, 2, 2, 3 ),
 ( 0.2500000000000002220, 0.2708333333333335369, 0.2916666666666669627, 0.3125000000000002776, 0.3333333333333335924 ),
 .UNSPECIFIED. ) 
 CURVE ( )  GEOMETRIC_REPRESENTATION_ITEM ( )  RATIONAL_B_SPLINE_CURVE ( ( 0.9999999999999992228, 0.9238795325112875156, 1.000000000000000000, 0.9238795325112867385, 1.000000000000000000, 0.9238795325112867385, 1.000000000000000000, 0.9238795325112857393, 1.000000000000001110 ) ) 
 REPRESENTATION_ITEM ( '' )  );
#6012 = DIRECTION ( 'NONE',  ( -1.000000000000000000, 0.000000000000000000, 0.000000000000000000 ) ) ;
#6013 = ORIENTED_EDGE ( 'NONE', *, *, #4258, .T. ) ;
#6014 = CARTESIAN_POINT ( 'NONE',  ( -80.00000000000002842, 46.51471862576140381, 9.985284746156354529 ) ) ;
#6015 = CARTESIAN_POINT ( 'NONE',  ( -74.37500000000000000, 30.00000000000000355, 4.592425496802573578E-15 ) ) ;
#6016 = LINE ( 'NONE', #8876, #3631 ) ;
#6017 = DIRECTION ( 'NONE',  ( 1.000000000000000000, -0.000000000000000000, -0.000000000000000000 ) ) ;
#6018 = ORIENTED_EDGE ( 'NONE', *, *, #9096, .T. ) ;
#6019 = CARTESIAN_POINT ( 'NONE',  ( -26.83355706786435491, 49.15565477916797477, 3.903659954469548055 ) ) ;
#6020 = CARTESIAN_POINT ( 'NONE',  ( -78.31250000409679046, 72.67766952966368876, 17.67766952966368521 ) ) ;
#6021 = FACE_OUTER_BOUND ( 'NONE', #4484, .T. ) ;
#6022 = ORIENTED_EDGE ( 'NONE', *, *, #4863, .F. ) ;
#6023 = CARTESIAN_POINT ( 'NONE',  ( 21.71463995357127885, 77.00007676519764743, -0.7273169618903911893 ) ) ;
#6024 = CARTESIAN_POINT ( 'NONE',  ( -75.87500000204838102, 65.69163855873949842, 25.81189881250000084 ) ) ;
#6025 = ORIENTED_EDGE ( 'NONE', *, *, #10309, .F. ) ;
#6026 = AXIS2_PLACEMENT_3D ( 'NONE', #9386, #1180, #1307 ) ;
#6027 = CARTESIAN_POINT ( 'NONE',  ( -75.21875000204839523, 29.18810118750000271, 4.741568889096522788E-15 ) ) ;
#6028 = ADVANCED_FACE ( 'NONE', ( #5110 ), #600, .F. ) ;
#6029 = CARTESIAN_POINT ( 'NONE',  ( -75.06471690546626974, 79.99999999999991473, 6.658686756724147671 ) ) ;
#6030 = CARTESIAN_POINT ( 'NONE',  ( 3.571755578639977724, 50.00000000000001421, 2.874253840576960811E-12 ) ) ;
#6031 = CARTESIAN_POINT ( 'NONE',  ( -15.71439516195324515, 54.99396298233272518, -0.006381203918883474741 ) ) ;
#6032 = SHAPE_REPRESENTATION_RELATIONSHIP ( 'NONE' , 'NONE' ,  #9454, #6721 ) ;
#6033 = CARTESIAN_POINT ( 'NONE',  ( -75.00000000000002842, 31.34658496415306672, -9.793415029090784429 ) ) ;
#6034 = ORIENTED_EDGE ( 'NONE', *, *, #8066, .F. ) ;
#6035 = CARTESIAN_POINT ( 'NONE',  ( -80.00000000000001421, 59.24264068711927678, -5.742637315201482906 ) ) ;
#6036 = EDGE_CURVE ( 'NONE', #9669, #5516, #7471, .T. ) ;
#6037 = CARTESIAN_POINT ( 'NONE',  ( -23.05849041873830885, 57.05917197429855037, 20.98589082339331569 ) ) ;
#6038 = VERTEX_POINT ( 'NONE', #7802 ) ;
#6039 = CARTESIAN_POINT ( 'NONE',  ( -6.363976791488124007, 62.08095487955036162, -19.78975161862042498 ) ) ;
#6040 = CARTESIAN_POINT ( 'NONE',  ( -23.40470529880934691, 56.37319246401821005, 13.98650468942532399 ) ) ;
#6041 = CARTESIAN_POINT ( 'NONE',  ( -79.25000000000000000, 55.00000000000000000, 24.99999999999999645 ) ) ;
#6042 = MECHANICAL_DESIGN_GEOMETRIC_PRESENTATION_REPRESENTATION (  '', ( #11181 ), #5456 ) ;
#6043 = CARTESIAN_POINT ( 'NONE',  ( -22.87671376304905735, 56.30254047324378064, 4.871888488731487499 ) ) ;
#6044 = EDGE_LOOP ( 'NONE', ( #7171, #3156, #4942, #4180 ) ) ;
#6045 = CARTESIAN_POINT ( 'NONE',  ( -78.12500000204838102, 44.30836144126050158, -25.81189881249999374 ) ) ;
#6046 = CARTESIAN_POINT ( 'NONE',  ( -80.00000000000002842, 46.51471862576140381, -1.499996628082201244 ) ) ;
#6047 = PRODUCT_DEFINITION_FORMATION_WITH_SPECIFIED_SOURCE ( 'ANY', '', #1748, .NOT_KNOWN. ) ;
#6049 = COLOUR_RGB ( '',0.8941176470588234615, 0.8941176470588234615, 0.8941176470588234615 ) ;
#6048 = CARTESIAN_POINT ( 'NONE',  ( -75.00000000000000000, 55.00000000000000000, 0.000000000000000000 ) ) ;
#6050 = DIRECTION ( 'NONE',  ( 0.000000000000000000, 1.000000000000000000, 0.000000000000000000 ) ) ;
#6051 = CARTESIAN_POINT ( 'NONE',  ( -55.24961050147904729, 61.18673322028157457, 3.306144321554119525 ) ) ;
#6052 = VERTEX_POINT ( 'NONE', #10544 ) ;
#6053 = CARTESIAN_POINT ( 'NONE',  ( -40.03064391692543467, 53.96877717286832876, -20.99202776130344361 ) ) ;
#6054 = CYLINDRICAL_SURFACE ( 'NONE', #11001, 20.00000000000000355 ) ;
#6055 = LINE ( 'NONE', #8739, #4664 ) ;
#6056 = CARTESIAN_POINT ( 'NONE',  ( -75.78125000204839523, 73.25176868561975141, 18.25176868561974075 ) ) ;
#6057 = EDGE_CURVE ( 'NONE', #7152, #11420, #6016, .T. ) ;
#6058 = FACE_OUTER_BOUND ( 'NONE', #7034, .T. ) ;
#6059 = CARTESIAN_POINT ( 'NONE',  ( -76.34375000204839523, 55.00000000000000000, -25.81189881249999729 ) ) ;
#6060 = ORIENTED_EDGE ( 'NONE', *, *, #5885, .F. ) ;
#6061 = CARTESIAN_POINT ( 'NONE',  ( -74.00000000409677625, 80.00000000000000000, -1.530808498934191324E-15 ) ) ;
#6062 = CARTESIAN_POINT ( 'NONE',  ( -80.00000000000000000, 55.00000000000000000, 22.00000000000000000 ) ) ;
#6063 = CARTESIAN_POINT ( 'NONE',  ( -80.00000000000000000, 55.00000000000000000, 0.000000000000000000 ) ) ;
#6064 = AXIS2_PLACEMENT_3D ( 'NONE', #1158, #4829, #1278 ) ;
#6065 = CARTESIAN_POINT ( 'NONE',  ( -18.45202553953894764, 65.80723110900194683, 18.02933743899848551 ) ) ;
#6066 = CARTESIAN_POINT ( 'NONE',  ( -76.15625000204838102, 80.81189881250000440, -1.580522963032174394E-15 ) ) ;
#6067 = CARTESIAN_POINT ( 'NONE',  ( -5.000000000000000000, 2.886751345948126879, -0.4465819873852047150 ) ) ;
#6068 = CARTESIAN_POINT ( 'NONE',  ( -78.00000000000001421, 46.51471862576140381, -6.985278002320760571 ) ) ;
#6069 = CONICAL_SURFACE ( 'NONE', #3953, 2.500000000000000000, 0.9599310885968755924 ) ;
#6070 = CARTESIAN_POINT ( 'NONE',  ( -79.53125000204838102, 55.00000000000000000, -25.81189881249999729 ) ) ;
#6071 = CARTESIAN_POINT ( 'NONE',  ( -74.84375000000000000, 65.35533905932737753, 24.99999999999999645 ) ) ;
#6072 = DIRECTION ( 'NONE',  ( 1.000000000000000000, 0.000000000000000000, 0.000000000000000000 ) ) ;
#6073 = ORIENTED_EDGE ( 'NONE', *, *, #4803, .F. ) ;
#6074 = EDGE_CURVE ( 'NONE', #7355, #4880, #8933, .T. ) ;
#6075 = AXIS2_PLACEMENT_3D ( 'NONE', #5967, #9604, #1396 ) ;
#6076 = CARTESIAN_POINT ( 'NONE',  ( 0.000000000000000000, -57.00000000000000000, 0.000000000000000000 ) ) ;
#6077 = VERTEX_POINT ( 'NONE', #3303 ) ;
#6078 = CARTESIAN_POINT ( 'NONE',  ( -40.24961187995522494, 55.68701082057744145, -6.984114430637439419 ) ) ;
#6079 = DIRECTION ( 'NONE',  ( -1.000000000000000000, -0.000000000000000000, -0.000000000000000000 ) ) ;
#6080 = FACE_OUTER_BOUND ( 'NONE', #9415, .T. ) ;
#6081 = CARTESIAN_POINT ( 'NONE',  ( 14.40112391949197779, 71.21751140778172839, 14.87572979763152681 ) ) ;
#6082 = CARTESIAN_POINT ( 'NONE',  ( -80.00000000000001421, 67.72792206135787296, -4.242637315201482906 ) ) ;
#6083 = AXIS2_PLACEMENT_3D ( 'NONE', #5912, #9616, #11391 ) ;
#6084 = ORIENTED_EDGE ( 'NONE', *, *, #11695, .F. ) ;
#6085 = CARTESIAN_POINT ( 'NONE',  ( -78.87500000204838102, 80.81189881250001861, 10.69163855873948599 ) ) ;
#6086 = ADVANCED_FACE ( 'NONE', ( #2347 ), #655, .F. ) ;
#6087 = LINE ( 'NONE', #8951, #9410 ) ;
#6088 = LINE ( 'NONE', #6929, #8463 ) ;
#6089 = CARTESIAN_POINT ( 'NONE',  ( 3.836827854034411178, 54.99596874490445231, -0.001874240170360355487 ) ) ;
#6090 = AXIS2_PLACEMENT_3D ( 'NONE', #4067, #11409, #339 ) ;
#6091 = DIRECTION ( 'NONE',  ( -1.000000000000000000, -0.000000000000000000, -0.000000000000000000 ) ) ;
#6092 = EDGE_LOOP ( 'NONE', ( #2547, #5229, #9215 ) ) ;
#6093 = PLANE ( 'NONE',  #6083 ) ;
#6094 = CARTESIAN_POINT ( 'NONE',  ( -43.78535878948660098, 60.10716095388539060, -20.39140800440753054 ) ) ;
#6095 = ORIENTED_EDGE ( 'NONE', *, *, #8065, .T. ) ;
#6096 = CARTESIAN_POINT ( 'NONE',  ( -41.67054327082605880, 55.00043308847957491, -21.02772144221139783 ) ) ;
#6097 = CARTESIAN_POINT ( 'NONE',  ( -15.46043787753367305, 69.01800930915912602, 1.830987716616894412 ) ) ;
#6098 = DIRECTION ( 'NONE',  ( -0.000000000000000000, -0.000000000000000000, -1.000000000000000000 ) ) ;
#6099 = EDGE_CURVE ( 'NONE', #8080, #6864, #4405, .T. ) ;
#6100 = AXIS2_PLACEMENT_3D ( 'NONE', #11253, #10366, #4679 ) ;
#6101 = EDGE_CURVE ( 'NONE', #7933, #3923, #1718, .T. ) ;
#6102 = ORIENTED_EDGE ( 'NONE', *, *, #10184, .F. ) ;
#6103 = CARTESIAN_POINT ( 'NONE',  ( -78.50000000204840944, 29.18810118750000981, 10.69163855873950020 ) ) ;
#6104 = CARTESIAN_POINT ( 'NONE',  ( 9.477680475861957277, 36.67126955513442255, 10.56417786655960356 ) ) ;
#6105 = CARTESIAN_POINT ( 'NONE',  ( 0.000000000000000000, 0.000000000000000000, -6.099999999999999645 ) ) ;
#6106 = CARTESIAN_POINT ( 'NONE',  ( 7.095683716263478047, 50.00000000000005684, 2.757939276259992832E-15 ) ) ;
#6107 = CARTESIAN_POINT ( 'NONE',  ( -41.24915659003143276, 52.95126970601198479, -6.742091308054726895 ) ) ;
#6108 = ORIENTED_EDGE ( 'NONE', *, *, #1182, .T. ) ;
#6109 = EDGE_CURVE ( 'NONE', #11411, #10886, #3066, .T. ) ;
#6110 = CARTESIAN_POINT ( 'NONE',  ( 14.18903896197797287, 52.25434875799748369, 21.02210295667673989 ) ) ;
#6111 = CARTESIAN_POINT ( 'NONE',  ( -83.00000000000000000, 55.00000000000000000, 0.000000000000000000 ) ) ;
#6112 = DIRECTION ( 'NONE',  ( 0.000000000000000000, 0.000000000000000000, 1.000000000000000000 ) ) ;
#6113 = DIRECTION ( 'NONE',  ( 0.000000000000000000, 0.000000000000000000, 1.000000000000000000 ) ) ;
#6114 = CARTESIAN_POINT ( 'NONE',  ( -74.56250000204839523, 80.81189881250001861, -10.69163855873949132 ) ) ;
#6115 = EDGE_LOOP ( 'NONE', ( #4026, #11004 ) ) ;
#6116 = CARTESIAN_POINT ( 'NONE',  ( -72.96875000409677625, 44.64466094067260826, -24.99999999999998934 ) ) ;
#6117 = FACE_OUTER_BOUND ( 'NONE', #4101, .T. ) ;
#6118 = CARTESIAN_POINT ( 'NONE',  ( -78.00000000000001421, 54.99999999999999289, -15.47055937655931501 ) ) ;
#6119 = CARTESIAN_POINT ( 'NONE',  ( 4.595919313165082620, 34.88938507153989832, -6.102095433906166377 ) ) ;
#6120 = VECTOR ( 'NONE', #2382, 1000.000000000000000 ) ;
#6121 = ORIENTED_EDGE ( 'NONE', *, *, #2288, .F. ) ;
#6122 = CARTESIAN_POINT ( 'NONE',  ( -77.00000000204839523, 29.18810118750000981, 10.69163855873950020 ) ) ;
#6123=STYLED_ITEM('',(#11895),#4740);
#6124 = DIRECTION ( 'NONE',  ( -1.000000000000000000, 0.000000000000000000, 0.000000000000000000 ) ) ;
#6125 = LINE ( 'NONE', #11430, #4169 ) ;
#6126 = CARTESIAN_POINT ( 'NONE',  ( -31.54809236465146682, 34.60179423563022283, 5.109615027512485419 ) ) ;
#6127 = DIRECTION ( 'NONE',  ( 0.000000000000000000, 0.000000000000000000, -1.000000000000000000 ) ) ;
#6128 = CIRCLE ( 'NONE', #8414, 1.500000000000001332 ) ;
#6129 = CARTESIAN_POINT ( 'NONE',  ( -76.90625000204838102, 29.18810118750000271, 4.741568889096522788E-15 ) ) ;
#6130 = CARTESIAN_POINT ( 'NONE',  ( -80.00000000000000000, 55.00000000000000000, 0.000000000000000000 ) ) ;
#6131 = VERTEX_POINT ( 'NONE', #2399 ) ;
#6132 = DIRECTION ( 'NONE',  ( 0.000000000000000000, 0.000000000000000000, 1.000000000000000000 ) ) ;
#6133 = ORIENTED_EDGE ( 'NONE', *, *, #9063, .F. ) ;
#6134 = CARTESIAN_POINT ( 'NONE',  ( -56.58242889277405396, 57.05108172246632137, 6.747627424565906473 ) ) ;
#6135 = DIRECTION ( 'NONE',  ( 0.000000000000000000, 1.000000000000000000, 0.000000000000000000 ) ) ;
#6136 = DIRECTION ( 'NONE',  ( 0.000000000000000000, 1.000000000000000000, 0.000000000000000000 ) ) ;
#6137 = CARTESIAN_POINT ( 'NONE',  ( -5.000000000000000000, 2.886751345948134428, -5.653418012614792154 ) ) ;
#6138 = AXIS2_PLACEMENT_3D ( 'NONE', #8036, #3484, #11674 ) ;
#6139 = DIRECTION ( 'NONE',  ( -1.000000000000000000, -0.000000000000000000, -0.000000000000000000 ) ) ;
#6140 = CARTESIAN_POINT ( 'NONE',  ( -73.53125000204838102, 55.00000000000000000, -25.81189881249999729 ) ) ;
#6141 = ORIENTED_EDGE ( 'NONE', *, *, #9822, .F. ) ;
#6142 = CARTESIAN_POINT ( 'NONE',  ( -75.68750000204839523, 65.69163855873949842, 25.81189881250000440 ) ) ;
#6143 = EDGE_CURVE ( 'NONE', #7749, #1776, #2726, .T. ) ;
#6144 = DIRECTION ( 'NONE',  ( 0.000000000000000000, 1.000000000000000000, 0.000000000000000000 ) ) ;
#6145 = VECTOR ( 'NONE', #3707, 1000.000000000000000 ) ;
#6146 = DIRECTION ( 'NONE',  ( 0.000000000000000000, 0.000000000000000000, 1.000000000000000000 ) ) ;
#6147 = CARTESIAN_POINT ( 'NONE',  ( -7.829838812692313077, 55.00327426656686214, -0.003007153403177842931 ) ) ;
#6148 = CARTESIAN_POINT ( 'NONE',  ( 0.000000000000000000, 0.000000000000000000, -6.099999999999999645 ) ) ;
#6149 = AXIS2_PLACEMENT_3D ( 'NONE', #1801, #1084, #900 ) ;
#6150 = ORIENTED_EDGE ( 'NONE', *, *, #956, .F. ) ;
#6151 = DIRECTION ( 'NONE',  ( -1.000000000000000000, -0.000000000000000000, -0.000000000000000000 ) ) ;
#6152 = VECTOR ( 'NONE', #3766, 1000.000000000000000 ) ;
#6153 = CARTESIAN_POINT ( 'NONE',  ( -60.69833702282029009, 56.03208645306531110, 20.99415308669729541 ) ) ;
#6154 = ORIENTED_EDGE ( 'NONE', *, *, #9135, .F. ) ;
#6155 = CARTESIAN_POINT ( 'NONE',  ( -26.14429485881147741, 44.41916384679638696, 18.36966221812192401 ) ) ;
#6156 = EDGE_CURVE ( 'NONE', #2139, #5990, #712, .T. ) ;
#6157 = CARTESIAN_POINT ( 'NONE',  ( -29.26205205118023400, 44.11983436432798555, 8.937929964154781359 ) ) ;
#6158 = CARTESIAN_POINT ( 'NONE',  ( -76.62500000204839523, 44.30836144126050158, -25.81189881249999374 ) ) ;
#6159 = AXIS2_PLACEMENT_3D ( 'NONE', #424, #11376, #3009 ) ;
#6160 = AXIS2_PLACEMENT_3D ( 'NONE', #1200, #9468, #9406 ) ;
#6161 = ORIENTED_EDGE ( 'NONE', *, *, #2392, .F. ) ;
#6162 = CARTESIAN_POINT ( 'NONE',  ( -77.09375000204839523, 36.74823131438026280, 18.25176868561974786 ) ) ;
#6163 = CARTESIAN_POINT ( 'NONE',  ( 21.14436220910852882, 71.77416011014268804, 12.89076390558360075 ) ) ;
#6164 = CARTESIAN_POINT ( 'NONE',  ( 0.000000000000000000, 0.000000000000000000, 0.000000000000000000 ) ) ;
#6165 = ORIENTED_EDGE ( 'NONE', *, *, #3095, .F. ) ;
#6166 = PRODUCT_RELATED_PRODUCT_CATEGORY ( 'part', '', ( #7768 ) ) ;
#6167 = DIRECTION ( 'NONE',  ( -1.000000000000000000, -0.000000000000000000, -0.000000000000000000 ) ) ;
#6168 = CARTESIAN_POINT ( 'NONE',  ( 17.98255850431752378, 56.29716720365202320, 4.839784152412198281 ) ) ;
#6169 = CARTESIAN_POINT ( 'NONE',  ( -63.12525701739682660, 53.29900530425329208, 6.794067530835293134 ) ) ;
#6170 = EDGE_LOOP ( 'NONE', ( #2294, #5320 ) ) ;
#6171 = CARTESIAN_POINT ( 'NONE',  ( -64.47562408583945626, 38.19583575827792288, 12.92744520505189953 ) ) ;
#6172 = CLOSED_SHELL ( 'NONE', ( #3581, #9537, #7863, #5726, #11146, #11392, #11532, #7975, #4466, #1756, #1981, #5586, #10100 ) ) ;
#6173 = PLANE ( 'NONE',  #5473 ) ;
#6174 = CARTESIAN_POINT ( 'NONE',  ( 0.000000000000000000, 0.000000000000000000, -6.074599999999999334 ) ) ;
#6175 = CARTESIAN_POINT ( 'NONE',  ( 39.99999999999999289, 55.00000000000000000, 0.000000000000000000 ) ) ;
#6176 = CARTESIAN_POINT ( 'NONE',  ( -72.78125000204839523, 73.25176868561975141, 18.25176868561974075 ) ) ;
#6177 = EDGE_CURVE ( 'NONE', #7683, #7763, #4203, .T. ) ;
#6178 = EDGE_LOOP ( 'NONE', ( #9023, #10136 ) ) ;
#6179 = DIRECTION ( 'NONE',  ( 0.000000000000000000, 0.000000000000000000, -1.000000000000000000 ) ) ;
#6180 = CARTESIAN_POINT ( 'NONE',  ( -15.00000000000000000, -24.99999999999999645, 10.00000000000000000 ) ) ;
#6181 = CARTESIAN_POINT ( 'NONE',  ( -64.46266331143226580, 50.66432291203608429, 2.511714366154293110 ) ) ;
#6182 = CARTESIAN_POINT ( 'NONE',  ( -48.85567157503042779, 75.97628680226326026, -2.745941867523475466 ) ) ;
#6183 = ORIENTED_EDGE ( 'NONE', *, *, #6744, .F. ) ;
#6184 = CARTESIAN_POINT ( 'NONE',  ( -78.03125000204838102, 55.00000000000000000, -25.81189881249999729 ) ) ;
#6185 = SHAPE_REPRESENTATION ( 'Threaded Front Retaining Ring Collar', ( #4738 ), #3395 ) ;
#6186 = EDGE_CURVE ( 'NONE', #10943, #4583, #370, .T. ) ;
#6187 = CARTESIAN_POINT ( 'NONE',  ( -64.86454813115628326, 52.49943474288868828, 4.342307377127885282 ) ) ;
#6188 = EDGE_CURVE ( 'NONE', #9256, #2813, #3250, .T. ) ;
#6189 = LINE ( 'NONE', #2697, #7815 ) ;
#6190 = CARTESIAN_POINT ( 'NONE',  ( 9.009704903381607011, 51.94883714271350783, 3.974653465714529155 ) ) ;
#6191 = LINE ( 'NONE', #1389, #4818 ) ;
#6192 = CARTESIAN_POINT ( 'NONE',  ( -75.78125000204838102, 55.00000000000000000, 25.81189881249999729 ) ) ;
#6193 = CARTESIAN_POINT ( 'NONE',  ( 47.00000000000000000, 60.00000000000000000, 6.123233995736766282E-16 ) ) ;
#6194 = VERTEX_POINT ( 'NONE', #7977 ) ;
#6195 = DIRECTION ( 'NONE',  ( 0.000000000000000000, 0.000000000000000000, 1.000000000000000000 ) ) ;
#6196 = ORIENTED_EDGE ( 'NONE', *, *, #4635, .F. ) ;
#6197 = CARTESIAN_POINT ( 'NONE',  ( -43.16649569290354549, 58.90744599142516336, -5.853545488159599408 ) ) ;
#6198 = CARTESIAN_POINT ( 'NONE',  ( -78.68750000409679046, 72.67766952966368876, -17.67766952966368876 ) ) ;
#6199 = CARTESIAN_POINT ( 'NONE',  ( 0.4079457818577022499, -5.537975084925951919, -5.789399939901062275 ) ) ;
#6200 = DIRECTION ( 'NONE',  ( 0.000000000000000000, 1.000000000000000000, 0.000000000000000000 ) ) ;
#6201 = CARTESIAN_POINT ( 'NONE',  ( 52.99999999999999289, 58.53553390593273065, -3.535533905932738197 ) ) ;
#6202 = ORIENTED_EDGE ( 'NONE', *, *, #5579, .F. ) ;
#6203 = DIRECTION ( 'NONE',  ( -1.000000000000000000, -0.000000000000000000, -0.000000000000000000 ) ) ;
#6204 = CARTESIAN_POINT ( 'NONE',  ( -77.56250000204839523, 80.81189881250001861, -10.69163855873949132 ) ) ;
#6205 = CARTESIAN_POINT ( 'NONE',  ( -78.00000000000001421, 46.51471862576140381, -9.985278002320759683 ) ) ;
#6206 = DIRECTION ( 'NONE',  ( 0.000000000000000000, 1.000000000000000000, 0.000000000000000000 ) ) ;
#6207 = CARTESIAN_POINT ( 'NONE',  ( -2.569594468081864314, 55.00124604138196815, -0.01964962527651127611 ) ) ;
#6208 = FACE_OUTER_BOUND ( 'NONE', #5369, .T. ) ;
#6209 = ORIENTED_EDGE ( 'NONE', *, *, #4119, .T. ) ;
#6210 = CARTESIAN_POINT ( 'NONE',  ( -14.28778386244584730, 59.49503363445350601, 2.214355864345136649 ) ) ;
#6211 = AXIS2_PLACEMENT_3D ( 'NONE', #9034, #11106, #927 ) ;
#6212 = FACE_OUTER_BOUND ( 'NONE', #1870, .T. ) ;
#6213 = ORIENTED_EDGE ( 'NONE', *, *, #9946, .T. ) ;
#6214 = CARTESIAN_POINT ( 'NONE',  ( -39.94161417541742054, 48.86043757236269158, -20.20376349713652075 ) ) ;
#6215 = CARTESIAN_POINT ( 'NONE',  ( -48.87290492130438935, 67.21699422026077286, -7.042296406420784471 ) ) ;
#6216 = CARTESIAN_POINT ( 'NONE',  ( -76.06250000204839523, 80.81189881250001861, 10.69163855873948599 ) ) ;
#6217 = ORIENTED_EDGE ( 'NONE', *, *, #2426, .F. ) ;
#6218 = CARTESIAN_POINT ( 'NONE',  ( -74.09375000204839523, 36.74823131438026280, 18.25176868561974786 ) ) ;
#6219 = DIRECTION ( 'NONE',  ( -1.000000000000000000, -0.000000000000000000, -0.000000000000000000 ) ) ;
#6220 =( LENGTH_UNIT ( ) NAMED_UNIT ( * ) SI_UNIT ( .MILLI., .METRE. ) );
#6221 = B_SPLINE_CURVE_WITH_KNOTS ( 'NONE', 3,
 ( #11550, #10152, #991, #6402, #11828, #3694 ),
 .UNSPECIFIED., .F., .F.,
 ( 4, 2, 4 ),
 ( 0.005150343764683554260, 0.006610526168996385711, 0.008070708573309217163 ),
 .UNSPECIFIED. ) ;
#6222 = ORIENTED_EDGE ( 'NONE', *, *, #5685, .T. ) ;
#6223 = DIRECTION ( 'NONE',  ( -0.000000000000000000, -0.000000000000000000, -1.000000000000000000 ) ) ;
#6224 = ADVANCED_FACE ( 'NONE', ( #11614 ), #10714, .F. ) ;
#6225 = CARTESIAN_POINT ( 'NONE',  ( 3.000000000000000000, 3.673940397442059868E-16, -0.02539999999999996774 ) ) ;
#6226 = CARTESIAN_POINT ( 'NONE',  ( -2.907263427868458816, 55.00473918814381591, 0.01574419816156069629 ) ) ;
#6227 = ORIENTED_EDGE ( 'NONE', *, *, #6469, .F. ) ;
#6228 = CARTESIAN_POINT ( 'NONE',  ( 11.14427089164646212, 42.10785603453369674, 16.77510495723129580 ) ) ;
#6229 = CARTESIAN_POINT ( 'NONE',  ( -1.144262565995328940, 42.07883645215377300, -16.80394782698530065 ) ) ;
#6230 = B_SPLINE_CURVE_WITH_KNOTS ( 'NONE', 3,
 ( #811, #3750, #4480, #5439, #9087, #10870 ),
 .UNSPECIFIED., .F., .F.,
 ( 4, 2, 4 ),
 ( 0.005150343764683554260, 0.006610526168996384844, 0.008070708573309215428 ),
 .UNSPECIFIED. ) ;
#6231 = DIRECTION ( 'NONE',  ( -1.000000000000000000, -0.000000000000000000, -0.000000000000000000 ) ) ;
#6232 = DIRECTION ( 'NONE',  ( -1.000000000000000000, -0.000000000000000000, -0.000000000000000000 ) ) ;
#6233 = CARTESIAN_POINT ( 'NONE',  ( -5.000000000000000000, -2.886751345948134428, -5.653418012614792154 ) ) ;
#6234 = ORIENTED_EDGE ( 'NONE', *, *, #5482, .F. ) ;
#6235 = CARTESIAN_POINT ( 'NONE',  ( -71.46875000409677625, 44.64466094067260826, -24.99999999999998934 ) ) ;
#6236 = CARTESIAN_POINT ( 'NONE',  ( -15.00000000000000000, 55.00000000000000000, 20.00000000000000000 ) ) ;
#6237 = CARTESIAN_POINT ( 'NONE',  ( -3.000000000000000000, 0.000000000000000000, -0.8895714285714284575 ) ) ;
#6238 = AXIS2_PLACEMENT_3D ( 'NONE', #8837, #3259, #5361 ) ;
#6239 = VECTOR ( 'NONE', #6706, 1000.000000000000000 ) ;
#6240 = CARTESIAN_POINT ( 'NONE',  ( -40.92935782463053584, 57.05919160630219977, -20.93299540428984429 ) ) ;
#6241 = VERTEX_POINT ( 'NONE', #5281 ) ;
#6242 = PLANE ( 'NONE',  #1746 ) ;
#6243 = CARTESIAN_POINT ( 'NONE',  ( -52.81739729106450909, 59.99999999999995737, 0.3296920225250882797 ) ) ;
#6244 = ADVANCED_FACE ( 'NONE', ( #11435 ), #11273, .T. ) ;
#6245 = ORIENTED_EDGE ( 'NONE', *, *, #11646, .T. ) ;
#6246 = CARTESIAN_POINT ( 'NONE',  ( 52.99999999999999289, 93.00000000000000000, -4.898587196589397051E-16 ) ) ;
#6247 = CIRCLE ( 'NONE', #10901, 1.500000000000001332 ) ;
#6248 = CARTESIAN_POINT ( 'NONE',  ( 9.791712712594932810, 52.49391147245050604, 4.339007403345378933 ) ) ;
#6249 = CARTESIAN_POINT ( 'NONE',  ( -72.06435441788588037, 80.00000000000001421, 6.698726029249594482 ) ) ;
#6250 = CARTESIAN_POINT ( 'NONE',  ( -3.000000000000000888, 3.673940397442060854E-16, -6.099999999999997868 ) ) ;
#6251 = VERTEX_POINT ( 'NONE', #6250 ) ;
#6252 = LINE ( 'NONE', #4322, #11483 ) ;
#6253 = ORIENTED_EDGE ( 'NONE', *, *, #7338, .F. ) ;
#6254 = CARTESIAN_POINT ( 'NONE',  ( -3.791298217890237687, 56.29168220040835280, -4.841196073966652413 ) ) ;
#6255 = EDGE_CURVE ( 'NONE', #1817, #1114, #9877, .T. ) ;
#6256 = CARTESIAN_POINT ( 'NONE',  ( -4.703005425211010504, 59.71918865705544732, -13.18981795474766194 ) ) ;
#6257 = CARTESIAN_POINT ( 'NONE',  ( -78.78125000409680467, 65.35533905932737753, -24.99999999999999645 ) ) ;
#6258 = CARTESIAN_POINT ( 'NONE',  ( -83.00000000000000000, 55.00000000000000000, 20.00000000000000355 ) ) ;
#6259 = VECTOR ( 'NONE', #11166, 1000.000000000000000 ) ;
#6260 = CARTESIAN_POINT ( 'NONE',  ( 4.182066831946701591, -3.358985280702831755, -5.926062401966622595 ) ) ;
#6261 = CARTESIAN_POINT ( 'NONE',  ( -73.90625000204838102, 29.18810118750000271, 4.741568889096522788E-15 ) ) ;
#6262 = ORIENTED_EDGE ( 'NONE', *, *, #3608, .T. ) ;
#6263 = EDGE_CURVE ( 'NONE', #10429, #5239, #7663, .T. ) ;
#6264 = CARTESIAN_POINT ( 'NONE',  ( -74.00000000204840944, 44.30836144126053000, 25.81189881250000795 ) ) ;
#6265 = LINE ( 'NONE', #7991, #610 ) ;
#6266 = CARTESIAN_POINT ( 'NONE',  ( 0.000000000000000000, 0.000000000000000000, -6.099999999999999645 ) ) ;
#6267 = CARTESIAN_POINT ( 'NONE',  ( -41.09033010249994788, 54.99579895668967566, 0.009353565326378111486 ) ) ;
#6268 = DIRECTION ( 'NONE',  ( 1.000000000000000000, 0.000000000000000000, 0.000000000000000000 ) ) ;
#6269 = DIRECTION ( 'NONE',  ( 1.000000000000000000, 0.000000000000000000, 0.000000000000000000 ) ) ;
#6270 = VECTOR ( 'NONE', #2160, 1000.000000000000000 ) ;
#6271 = EDGE_LOOP ( 'NONE', ( #6968, #5391, #631, #8483 ) ) ;
#6272 = DIRECTION ( 'NONE',  ( -1.000000000000000000, -0.000000000000000000, -0.000000000000000000 ) ) ;
#6273 = AXIS2_PLACEMENT_3D ( 'NONE', #2637, #709, #4443 ) ;
#6274 = CARTESIAN_POINT ( 'NONE',  ( -56.63607177307330431, 69.12418599258134577, 15.58301102096070245 ) ) ;
#6275 = ORIENTED_EDGE ( 'NONE', *, *, #11517, .F. ) ;
#6276 = CARTESIAN_POINT ( 'NONE',  ( -53.03060745306661516, 74.78972051499107465, 7.080976978603892746 ) ) ;
#6277 = CARTESIAN_POINT ( 'NONE',  ( -75.00000000000000000, 55.00000000000000000, 25.00000000000000355 ) ) ;
#6278 = AXIS2_PLACEMENT_3D ( 'NONE', #250, #6625, #10253 ) ;
#6279 = ORIENTED_EDGE ( 'NONE', *, *, #9241, .F. ) ;
#6280 = CARTESIAN_POINT ( 'NONE',  ( -72.59375000204838102, 36.74823131438026280, 18.25176868561974786 ) ) ;
#6281 = LINE ( 'NONE', #9025, #2016 ) ;
#6282 = FILL_AREA_STYLE ('',( #7064 ) ) ;
#6283 = CARTESIAN_POINT ( 'NONE',  ( 14.99999999999999645, 5.000000000000000000, 30.00000000000000711 ) ) ;
#6284 = CARTESIAN_POINT ( 'NONE',  ( 17.20429921762959324, 55.65812106999769782, 4.967195391103087942 ) ) ;
#6285 = CARTESIAN_POINT ( 'NONE',  ( 1.871464948240592063, 55.00332452672969907, 0.001624608827728054976 ) ) ;
#6286 = EDGE_LOOP ( 'NONE', ( #448, #971, #7179, #6253 ) ) ;
#6287 = CARTESIAN_POINT ( 'NONE',  ( -0.5223957761089466079, 44.43543377721479004, -18.33034268388519195 ) ) ;
#6288 = CARTESIAN_POINT ( 'NONE',  ( -17.27494751259140315, 73.62640980466187557, 9.944421848179040069 ) ) ;
#6289 = FILL_AREA_STYLE_COLOUR ( '', #2592 ) ;
#6290 = DIRECTION ( 'NONE',  ( -0.000000000000000000, -0.000000000000000000, 1.000000000000000000 ) ) ;
#6291 = CARTESIAN_POINT ( 'NONE',  ( -78.00000000000002842, 54.99999999999998579, 8.485284746156354529 ) ) ;
#6292 = EDGE_LOOP ( 'NONE', ( #9083, #502, #7922, #11618 ) ) ;
#6293 = EDGE_CURVE ( 'NONE', #1850, #11230, #4019, .T. ) ;
#6294 = CARTESIAN_POINT ( 'NONE',  ( -78.00000000000001421, 71.97056274847716395, 1.500003371917795425 ) ) ;
#6295 = DIRECTION ( 'NONE',  ( 0.000000000000000000, -0.000000000000000000, 1.000000000000000000 ) ) ;
#6296 = FACE_OUTER_BOUND ( 'NONE', #2671, .T. ) ;
#6297 = CIRCLE ( 'NONE', #11021, 1.500000000000001332 ) ;
#6298 = ORIENTED_EDGE ( 'NONE', *, *, #6099, .F. ) ;
#6299 = LINE ( 'NONE', #6471, #6931 ) ;
#6300 = FACE_OUTER_BOUND ( 'NONE', #10187, .T. ) ;
#6301 = ADVANCED_FACE ( 'NONE', ( #5455 ), #4983, .F. ) ;
#6302 = ORIENTED_EDGE ( 'NONE', *, *, #2580, .T. ) ;
#6303 = FACE_OUTER_BOUND ( 'NONE', #2617, .T. ) ;
#6304 = CARTESIAN_POINT ( 'NONE',  ( -70.34104699118840642, 33.99562393659799397, 0.006612473344882377653 ) ) ;
#6305 = CARTESIAN_POINT ( 'NONE',  ( -74.37500000204838102, 65.69163855873949842, 25.81189881250000440 ) ) ;
#6306 = CARTESIAN_POINT ( 'NONE',  ( -78.50000000204840944, 29.18810118750000981, 10.69163855873950020 ) ) ;
#6307 = ORIENTED_EDGE ( 'NONE', *, *, #6830, .T. ) ;
#6308 = CARTESIAN_POINT ( 'NONE',  ( -76.43750000204839523, 44.30836144126050158, -25.81189881249999374 ) ) ;
#6309 = ORIENTED_EDGE ( 'NONE', *, *, #6385, .T. ) ;
#6310 = CARTESIAN_POINT ( 'NONE',  ( -4.177541715523163113, 56.60546344811582742, -4.746664548824306884 ) ) ;
#6311 = CARTESIAN_POINT ( 'NONE',  ( -15.49691217297365142, 66.69002736867275871, 7.815521802502809479 ) ) ;
#6312 = CARTESIAN_POINT ( 'NONE',  ( -77.09375000204839523, 55.00000000000000000, 25.81189881249999729 ) ) ;
#6313 = CARTESIAN_POINT ( 'NONE',  ( -15.00000000000000000, 39.99999999999999289, 20.00000000000000000 ) ) ;
#6314 = ADVANCED_FACE ( 'NONE', ( #9939 ), #5938, .T. ) ;
#6315 = CARTESIAN_POINT ( 'NONE',  ( -33.76207074264209496, 50.00000000000002842, -7.785926851161516095E-15 ) ) ;
#6316 = CIRCLE ( 'NONE', #3426, 3.000000000000000000 ) ;
#6317 = CARTESIAN_POINT ( 'NONE',  ( -74.00000000204838102, 29.18810118750000981, 10.69163855873950020 ) ) ;
#6318 = AXIS2_PLACEMENT_3D ( 'NONE', #1494, #1661, #7015 ) ;
#6319 = ORIENTED_EDGE ( 'NONE', *, *, #6109, .T. ) ;
#6320 = SURFACE_STYLE_FILL_AREA ( #837 ) ;
#6321 = CARTESIAN_POINT ( 'NONE',  ( -75.96875000409677625, 44.64466094067260826, -24.99999999999998934 ) ) ;
#6322 = CARTESIAN_POINT ( 'NONE',  ( -80.00000000000000000, 54.99999999999999289, 3.371917797062584654E-06 ) ) ;
#6323 = EDGE_CURVE ( 'NONE', #11278, #6597, #8037, .T. ) ;
#6324 = EDGE_CURVE ( 'NONE', #3266, #9403, #2266, .T. ) ;
#6325 = DIRECTION ( 'NONE',  ( -1.000000000000000000, 0.000000000000000000, 0.000000000000000000 ) ) ;
#6326 = CARTESIAN_POINT ( 'NONE',  ( -45.57393268948897713, 54.97518271910073651, 0.008495404467763291445 ) ) ;
#6327 = ITEM_DEFINED_TRANSFORMATION ( 'NONE', 'NONE', #10027,  #4738 ) ;
#6328 = AXIS2_PLACEMENT_3D ( 'NONE', #4320, #5228, #11494 ) ;
#6329 = DIRECTION ( 'NONE',  ( 0.000000000000000000, 0.000000000000000000, 1.000000000000000000 ) ) ;
#6330 = ADVANCED_FACE ( 'NONE', ( #9036 ), #8307, .F. ) ;
#6331 = CARTESIAN_POINT ( 'NONE',  ( -5.000000000000000000, -2.886751345948133540, -6.099999999999999645 ) ) ;
#6332 = CARTESIAN_POINT ( 'NONE',  ( -61.00490302436042356, 55.00059028654953153, 21.02810969917934614 ) ) ;
#6333 = ORIENTED_EDGE ( 'NONE', *, *, #7566, .T. ) ;
#6334 = CARTESIAN_POINT ( 'NONE',  ( -43.99614436914441029, 63.04465853171391387, -19.42287488623002290 ) ) ;
#6335 = CARTESIAN_POINT ( 'NONE',  ( -78.68750000204838102, 44.30836144126053000, 25.81189881250000795 ) ) ;
#6336 = ORIENTED_EDGE ( 'NONE', *, *, #3731, .F. ) ;
#6337 = CARTESIAN_POINT ( 'NONE',  ( -74.46875000204839523, 73.25176868561975141, 18.25176868561974075 ) ) ;
#6338 = CARTESIAN_POINT ( 'NONE',  ( -21.05849041552747281, 57.05917194494736577, 20.98221040122819403 ) ) ;
#6339 = CIRCLE ( 'NONE', #9379, 9.999999999999987566 ) ;
#6340 = EDGE_LOOP ( 'NONE', ( #9997, #1248, #4796, #3548 ) ) ;
#6341 = AXIS2_PLACEMENT_3D ( 'NONE', #7591, #4835, #7534 ) ;
#6342 = FACE_BOUND ( 'NONE', #9069, .T. ) ;
#6343 = CARTESIAN_POINT ( 'NONE',  ( -62.54147003350998801, 53.97158195009890136, 6.934912854774474944 ) ) ;
#6344 = ORIENTED_EDGE ( 'NONE', *, *, #2060, .T. ) ;
#6345 = CARTESIAN_POINT ( 'NONE',  ( 5.070642430964857894, 34.06762781005689078, -2.059172530961658865 ) ) ;
#6346 = VECTOR ( 'NONE', #3522, 1000.000000000000000 ) ;
#6347 = AXIS2_PLACEMENT_3D ( 'NONE', #3248, #3490, #10550 ) ;
#6348 = CARTESIAN_POINT ( 'NONE',  ( -22.50647595179652072, 59.12487335784310005, 20.69694904210189179 ) ) ;
#6349 = CARTESIAN_POINT ( 'NONE',  ( -78.00000000000002842, 42.27207793864211283, 12.72792543327562775 ) ) ;
#6350 = CARTESIAN_POINT ( 'NONE',  ( -78.00000000000000000, 54.99999999999999289, -1.499996628082203021 ) ) ;
#6351 = CARTESIAN_POINT ( 'NONE',  ( -2.712167343862823987, -4.207632145829752979, -6.099999999999999645 ) ) ;
#6352 = ORIENTED_EDGE ( 'NONE', *, *, #6789, .T. ) ;
#6353 = DIRECTION ( 'NONE',  ( -1.000000000000000000, 0.000000000000000000, 0.000000000000000000 ) ) ;
#6354 = CARTESIAN_POINT ( 'NONE',  ( -43.04772718432226952, 54.99964267904652360, 0.005532449227661951838 ) ) ;
#6355 = CARTESIAN_POINT ( 'NONE',  ( -35.67858024924570515, 51.94572111605872777, -3.972273510035316146 ) ) ;
#6356 = ORIENTED_EDGE ( 'NONE', *, *, #10786, .F. ) ;
#6357 = CIRCLE ( 'NONE', #2714, 4.999999999999984013 ) ;
#6358 = AXIS2_PLACEMENT_3D ( 'NONE', #8874, #2460, #6127 ) ;
#6359 = CARTESIAN_POINT ( 'NONE',  ( -5.000000000000000000, 2.886751345948126879, -6.099999999999999645 ) ) ;
#6360 = CARTESIAN_POINT ( 'NONE',  ( -55.53658087589213466, 59.34025876743092454, 2.504133036876110996 ) ) ;
#6361 = EDGE_LOOP ( 'NONE', ( #10492, #10043, #4727, #455 ) ) ;
#6362 = EDGE_CURVE ( 'NONE', #541, #10278, #5947, .T. ) ;
#6363 = LINE ( 'NONE', #3651, #10285 ) ;
#6364 = CARTESIAN_POINT ( 'NONE',  ( -11.57142270279487306, 60.00000000000001421, -4.065933922700817035E-15 ) ) ;
#6365 = CARTESIAN_POINT ( 'NONE',  ( 22.23809523809524435, 59.99999999999998579, 0.000000000000000000 ) ) ;
#6366 = CARTESIAN_POINT ( 'NONE',  ( -78.50000000204840944, 29.18810118750000981, 10.69163855873950020 ) ) ;
#6367 = AXIS2_PLACEMENT_3D ( 'NONE', #669, #727, #4399 ) ;
#6368 = CARTESIAN_POINT ( 'NONE',  ( -77.18750000204838102, 44.30836144126053000, 25.81189881250000795 ) ) ;
#6369 = ORIENTED_EDGE ( 'NONE', *, *, #3354, .F. ) ;
#6370 = CARTESIAN_POINT ( 'NONE',  ( -78.96875000204839523, 80.81189881250000440, -1.580522963032174394E-15 ) ) ;
#6371 = ORIENTED_EDGE ( 'NONE', *, *, #2946, .T. ) ;
#6372 = CARTESIAN_POINT ( 'NONE',  ( 22.22529492952226704, 77.41112953092405746, 11.08543588549235182 ) ) ;
#6373 = CARTESIAN_POINT ( 'NONE',  ( 4.036346099538457466, 42.32158391892036775, -5.996328608354988710 ) ) ;
#6374 = CARTESIAN_POINT ( 'NONE',  ( -75.03125000204839523, 36.74823131438024859, -18.25176868561973720 ) ) ;
#6375 = LINE ( 'NONE', #10841, #2619 ) ;
#6376 = FACE_OUTER_BOUND ( 'NONE', #7651, .T. ) ;
#6377 = ORIENTED_EDGE ( 'NONE', *, *, #7055, .F. ) ;
#6378 = LINE ( 'NONE', #2537, #10798 ) ;
#6379 = CARTESIAN_POINT ( 'NONE',  ( -77.37500000409677625, 55.00000000000000000, -24.99999999999999645 ) ) ;
#6380 = FACE_OUTER_BOUND ( 'NONE', #3840, .T. ) ;
#6381 = CARTESIAN_POINT ( 'NONE',  ( -36.24052534987266938, 55.00849635663053050, 0.02481536697055203647 ) ) ;
#6382 = CARTESIAN_POINT ( 'NONE',  ( -15.00000000000000355, 5.000000000000000000, -29.99999999999999289 ) ) ;
#6383 = FACE_OUTER_BOUND ( 'NONE', #7981, .T. ) ;
#6384 = VERTEX_POINT ( 'NONE', #1721 ) ;
#6385 = EDGE_CURVE ( 'NONE', #1831, #5363, #8995, .T. ) ;
#6386 = DIRECTION ( 'NONE',  ( 0.000000000000000000, 1.000000000000000000, 0.000000000000000000 ) ) ;
#6387 = ORIENTED_EDGE ( 'NONE', *, *, #10002, .T. ) ;
#6388 = CARTESIAN_POINT ( 'NONE',  ( 3.737309610555803463, 34.06887424008940712, -2.059134394038261817 ) ) ;
#6389 =( BOUNDED_CURVE ( )  B_SPLINE_CURVE ( 2, ( #10071, #2053, #5537, #5727, #7398, #1933, #8474, #4695, #6441 ),
 .UNSPECIFIED., .F., .T. ) 
 B_SPLINE_CURVE_WITH_KNOTS ( ( 3, 2, 2, 2, 3 ),
 ( 0.5000000000000004441, 0.5208333333333338144, 0.5416666666666670737, 0.5625000000000004441, 0.5833333333333338144 ),
 .UNSPECIFIED. ) 
 CURVE ( )  GEOMETRIC_REPRESENTATION_ITEM ( )  RATIONAL_B_SPLINE_CURVE ( ( 0.9999999999999983347, 0.9238795325112884038, 1.000000000000000000, 0.9238795325112867385, 1.000000000000000000, 0.9238795325112867385, 1.000000000000000000, 0.9238795325112850731, 1.000000000000001554 ) ) 
 REPRESENTATION_ITEM ( '' )  );
#6390 = CARTESIAN_POINT ( 'NONE',  ( -73.53125000204838102, 55.00000000000000000, -25.81189881249999729 ) ) ;
#6391 = EDGE_LOOP ( 'NONE', ( #281, #9197, #5981, #7424, #9340, #10052 ) ) ;
#6392 = CARTESIAN_POINT ( 'NONE',  ( -75.21875000204839523, 36.74823131438024859, -18.25176868561973720 ) ) ;
#6393 = CARTESIAN_POINT ( 'NONE',  ( -29.54809237377008202, 34.60091625530366599, 5.109976345715927515 ) ) ;
#6394 =( NAMED_UNIT ( * ) PLANE_ANGLE_UNIT ( ) SI_UNIT ( $, .RADIAN. ) );
#6395 = ADVANCED_FACE ( 'NONE', ( #10035 ), #5442, .F. ) ;
#6396 = ORIENTED_EDGE ( 'NONE', *, *, #2276, .F. ) ;
#6397 = DIRECTION ( 'NONE',  ( 0.000000000000000000, 1.000000000000000000, 0.000000000000000000 ) ) ;
#6398 = CARTESIAN_POINT ( 'NONE',  ( -0.7638017253321776057, 55.00780231169513002, 0.009546663813864672207 ) ) ;
#6399 = ORIENTED_EDGE ( 'NONE', *, *, #7701, .F. ) ;
#6400 = CARTESIAN_POINT ( 'NONE',  ( -16.49360055079280940, 72.53723377933144434, 11.72566733603474098 ) ) ;
#6401 = CARTESIAN_POINT ( 'NONE',  ( -34.17314261869798742, 34.29999169977881479, -4.109493429249395646 ) ) ;
#6402 = CARTESIAN_POINT ( 'NONE',  ( 5.000000000000000000, -0.9724665692850895660, -0.04193043885209624122 ) ) ;
#6403 = CARTESIAN_POINT ( 'NONE',  ( -80.00000000000000000, 55.00000000000000000, 0.000000000000000000 ) ) ;
#6404 = CARTESIAN_POINT ( 'NONE',  ( 0.000000000000000000, -30.00000000000000000, 0.000000000000000000 ) ) ;
#6405 = ORIENTED_EDGE ( 'NONE', *, *, #5820, .T. ) ;
#6406 = CARTESIAN_POINT ( 'NONE',  ( -70.93935441986302237, 79.99999999999998579, 6.698726263377742463 ) ) ;
#6407 = CARTESIAN_POINT ( 'NONE',  ( -43.33118549350501780, 55.00018389033358091, -0.001986509158416555499 ) ) ;
#6408 = CARTESIAN_POINT ( 'NONE',  ( -41.12561409036811000, 56.30289684387001614, -4.871785110082141657 ) ) ;
#6409 = DIRECTION ( 'NONE',  ( -1.000000000000000000, 0.000000000000000000, -0.000000000000000000 ) ) ;
#6410 = PLANE ( 'NONE',  #6449 ) ;
#6411 = EDGE_LOOP ( 'NONE', ( #3971, #104 ) ) ;
#6412 = EDGE_CURVE ( 'NONE', #10937, #8985, #180, .T. ) ;
#6413 = FACE_OUTER_BOUND ( 'NONE', #11490, .T. ) ;
#6414 = CARTESIAN_POINT ( 'NONE',  ( -29.48439297115004010, 51.23129068170470646, 3.302108576988587174 ) ) ;
#6415 = FACE_OUTER_BOUND ( 'NONE', #713, .T. ) ;
#6416 = CARTESIAN_POINT ( 'NONE',  ( -8.886150220881933848, 67.92913895864731444, -21.40220125730746759 ) ) ;
#6417 = B_SPLINE_CURVE_WITH_KNOTS ( 'NONE', 1,
 ( #9824, #6070 ),
 .UNSPECIFIED., .F., .F.,
 ( 2, 2 ),
 ( 0.000000000000000000, 1.000000000000000000 ),
 .UNSPECIFIED. ) ;
#6418 = CARTESIAN_POINT ( 'NONE',  ( -76.06250000204839523, 80.81189881250001861, 10.69163855873948599 ) ) ;
#6419 = AXIS2_PLACEMENT_3D ( 'NONE', #4344, #4220, #1696 ) ;
#6420 = ORIENTED_EDGE ( 'NONE', *, *, #10682, .T. ) ;
#6421 = CARTESIAN_POINT ( 'NONE',  ( -76.53125000204839523, 36.74823131438024859, -18.25176868561973720 ) ) ;
#6422 = ORIENTED_EDGE ( 'NONE', *, *, #5708, .T. ) ;
#6423 = CARTESIAN_POINT ( 'NONE',  ( 18.68839539025461605, 74.55286672756655264, 15.58206179569618577 ) ) ;
#6424 = CARTESIAN_POINT ( 'NONE',  ( 12.12709278872420526, 46.41256629213580709, 11.17685062095174331 ) ) ;
#6425 = CARTESIAN_POINT ( 'NONE',  ( -77.46875000204839523, 80.81189881250000440, -1.580522963032174394E-15 ) ) ;
#6426 = CARTESIAN_POINT ( 'NONE',  ( -78.68750000000002842, 37.32233047033633966, -17.67766952966366034 ) ) ;
#6427 = AXIS2_PLACEMENT_3D ( 'NONE', #10906, #724, #9060 ) ;
#6428 = CARTESIAN_POINT ( 'NONE',  ( 23.00000000000000000, 76.00000000000000000, 0.000000000000000000 ) ) ;
#6429 = ORIENTED_EDGE ( 'NONE', *, *, #11121, .F. ) ;
#6430 = EDGE_CURVE ( 'NONE', #8424, #11218, #1775, .T. ) ;
#6431 = CARTESIAN_POINT ( 'NONE',  ( -72.50000000204839523, 44.30836144126053000, 25.81189881250000795 ) ) ;
#6432 = DIRECTION ( 'NONE',  ( -1.000000000000000000, -0.000000000000000000, -0.000000000000000000 ) ) ;
#6433 = CARTESIAN_POINT ( 'NONE',  ( -51.57640054972269184, 55.00858919803477676, 0.004561873522476029598 ) ) ;
#6434 = ITEM_DEFINED_TRANSFORMATION ( 'NONE', 'NONE', #6238,  #4738 ) ;
#6435 = CARTESIAN_POINT ( 'NONE',  ( -20.82524276125487361, 76.25657222871954843, 5.681780444169967303 ) ) ;
#6436 = CIRCLE ( 'NONE', #4331, 1.500000000000001332 ) ;
#6437 = CARTESIAN_POINT ( 'NONE',  ( -11.57142270279487306, 60.00000000000001421, -4.065933922700817035E-15 ) ) ;
#6438 = ORIENTED_EDGE ( 'NONE', *, *, #3551, .T. ) ;
#6439 = VECTOR ( 'NONE', #248, 1000.000000000000000 ) ;
#6440 = ADVANCED_FACE ( 'NONE', ( #3580 ), #2685, .F. ) ;
#6441 = CARTESIAN_POINT ( 'NONE',  ( -73.62500000409677625, 55.00000000000000000, 24.99999999999999645 ) ) ;
#6442 = ORIENTED_EDGE ( 'NONE', *, *, #7630, .F. ) ;
#6443 = CARTESIAN_POINT ( 'NONE',  ( -7.030643242133587378, 62.08114452727563304, -19.79025909736091648 ) ) ;
#6444 = CARTESIAN_POINT ( 'NONE',  ( -78.03125000204839523, 36.74823131438024859, -18.25176868561973720 ) ) ;
#6445 = AXIS2_PLACEMENT_3D ( 'NONE', #4949, #8605, #7705 ) ;
#6446 = ORIENTED_EDGE ( 'NONE', *, *, #2574, .F. ) ;
#6447 = CARTESIAN_POINT ( 'NONE',  ( -76.06250000204839523, 80.81189881250001861, 10.69163855873948599 ) ) ;
#6448 = CARTESIAN_POINT ( 'NONE',  ( -5.030643890195627854, 62.08057558410310861, -19.78873666113293694 ) ) ;
#6449 = AXIS2_PLACEMENT_3D ( 'NONE', #5507, #9329, #10042 ) ;
#6450 = CARTESIAN_POINT ( 'NONE',  ( -67.52720549794999272, 34.02364409886038743, 2.748840581154547102 ) ) ;
#6451 = VERTEX_POINT ( 'NONE', #2746 ) ;
#6452 = LINE ( 'NONE', #4420, #4196 ) ;
#6453 = EDGE_CURVE ( 'NONE', #5404, #5247, #9979, .T. ) ;
#6454 = CARTESIAN_POINT ( 'NONE',  ( 1.697306494461763959, 35.98764835359665426, -8.991780390316415961 ) ) ;
#6455 = VERTEX_POINT ( 'NONE', #3697 ) ;
#6456 = EDGE_CURVE ( 'NONE', #1322, #11030, #378, .T. ) ;
#6457 = CARTESIAN_POINT ( 'NONE',  ( -44.50647629921198245, 66.71846839581321831, -17.55227556201471018 ) ) ;
#6458 = EDGE_CURVE ( 'NONE', #7798, #11523, #9205, .T. ) ;
#6459 = AXIS2_PLACEMENT_3D ( 'NONE', #7838, #11467, #3109 ) ;
#6460 = CARTESIAN_POINT ( 'NONE',  ( -18.69730990872651333, 70.57397863033268948, 14.11552877426516339 ) ) ;
#6461 = CARTESIAN_POINT ( 'NONE',  ( -73.62500000409677625, 55.00000000000000000, 24.99999999999999645 ) ) ;
#6462 = DIRECTION ( 'NONE',  ( -1.000000000000000000, 0.000000000000000000, 0.000000000000000000 ) ) ;
#6463 = DIRECTION ( 'NONE',  ( -1.000000000000000000, 0.000000000000000000, 0.000000000000000000 ) ) ;
#6464 = CARTESIAN_POINT ( 'NONE',  ( -78.00000000000002842, 42.27207793864211283, 12.72792543327562775 ) ) ;
#6465 = ORIENTED_EDGE ( 'NONE', *, *, #2183, .F. ) ;
#6466 = CARTESIAN_POINT ( 'NONE',  ( 0.000000000000000000, -30.00000000000000000, 0.000000000000000000 ) ) ;
#6467 = CARTESIAN_POINT ( 'NONE',  ( -59.09748447831353246, 54.99655739826935275, -0.01220661389743049260 ) ) ;
#6468 = CARTESIAN_POINT ( 'NONE',  ( -37.04640917235918351, 52.93602743192931115, -4.557080977652598897 ) ) ;
#6469 = EDGE_CURVE ( 'NONE', #11373, #11066, #3448, .T. ) ;
#6470 = ADVANCED_FACE ( 'NONE', ( #2799 ), #7250, .F. ) ;
#6471 = CARTESIAN_POINT ( 'NONE',  ( -2.500000000000000000, 3.061616997868383141E-16, -6.099999999999999645 ) ) ;
#6472 = AXIS2_PLACEMENT_3D ( 'NONE', #4102, #5982, #6991 ) ;
#6473 = EDGE_CURVE ( 'NONE', #9349, #2528, #10126, .T. ) ;
#6474 = FACE_BOUND ( 'NONE', #8910, .T. ) ;
#6475 = ORIENTED_EDGE ( 'NONE', *, *, #2866, .T. ) ;
#6476 = CARTESIAN_POINT ( 'NONE',  ( -78.00000000000000000, 54.99999999999999289, 3.371917797062584654E-06 ) ) ;
#6477 = CARTESIAN_POINT ( 'NONE',  ( 9.999999999999994671, 0.000000000000000000, -10.00000000000000000 ) ) ;
#6478 = CARTESIAN_POINT ( 'NONE',  ( -83.00000000000000000, 55.00000000000000000, -20.00000000000000355 ) ) ;
#6479 = CARTESIAN_POINT ( 'NONE',  ( -73.06250000204840944, 80.81189881250001861, 10.69163855873948599 ) ) ;
#6480 = CARTESIAN_POINT ( 'NONE',  ( -76.62500000204839523, 44.30836144126050158, -25.81189881249999374 ) ) ;
#6481 = AXIS2_PLACEMENT_3D ( 'NONE', #4081, #11371, #3180 ) ;
#6482 = EDGE_LOOP ( 'NONE', ( #8136, #2153 ) ) ;
#6483 = CARTESIAN_POINT ( 'NONE',  ( -77.56250000204839523, 80.81189881250001861, -10.69163855873949132 ) ) ;
#6484 = VERTEX_POINT ( 'NONE', #930 ) ;
#6485 = CARTESIAN_POINT ( 'NONE',  ( 17.86907162826477702, 73.91589606910815746, 16.34925201472697864 ) ) ;
#6486 = CARTESIAN_POINT ( 'NONE',  ( -9.071371961462144640, 67.39181373483076243, -6.619190081737647446 ) ) ;
#6487 = CARTESIAN_POINT ( 'NONE',  ( -78.87500000204839523, 80.81189881250000440, 10.69163855873948243 ) ) ;
#6488 = CARTESIAN_POINT ( 'NONE',  ( -75.00000000000001421, 70.68788533342120672, -20.24596063305270377 ) ) ;
#6489 = FACE_OUTER_BOUND ( 'NONE', #4711, .T. ) ;
#6490 = EDGE_LOOP ( 'NONE', ( #315, #4297, #11515, #4464 ) ) ;
#6491 = CARTESIAN_POINT ( 'NONE',  ( -78.00000000000001421, 54.99999999999998579, -6.985278002320760571 ) ) ;
#6492 = CARTESIAN_POINT ( 'NONE',  ( -71.46875000204838102, 80.81189881250000440, -1.580522963032174394E-15 ) ) ;
#6493 = VECTOR ( 'NONE', #459, 1000.000000000000000 ) ;
#6494 = CARTESIAN_POINT ( 'NONE',  ( -78.00000000000001421, 50.75735931288069480, -4.242637315201482906 ) ) ;
#6495 = CARTESIAN_POINT ( 'NONE',  ( -33.90726341901891772, 55.01734440879120314, 0.01967313780937999038 ) ) ;
#6496 = PRODUCT_CONTEXT ( 'NONE', #2098, 'mechanical' ) ;
#6497 = DIRECTION ( 'NONE',  ( 0.000000000000000000, 1.000000000000000000, 0.000000000000000000 ) ) ;
#6498 = CARTESIAN_POINT ( 'NONE',  ( -78.00000000000001421, 50.75735931288069480, -5.742637315201482906 ) ) ;
#6499 = VECTOR ( 'NONE', #11345, 1000.000000000000000 ) ;
#6500 = ORIENTED_EDGE ( 'NONE', *, *, #9822, .T. ) ;
#6501 = CARTESIAN_POINT ( 'NONE',  ( 10.20138320063666981, 50.66135930820338018, 2.506893722508881428 ) ) ;
#6502 = LINE ( 'NONE', #8409, #1535 ) ;
#6503 = EDGE_LOOP ( 'NONE', ( #3186, #8786, #9567, #6776 ) ) ;
#6504 = EDGE_CURVE ( 'NONE', #5852, #7713, #88, .T. ) ;
#6505 = CARTESIAN_POINT ( 'NONE',  ( 8.189038476963473201, 38.19597440261895827, 12.92108669627241646 ) ) ;
#6506 = CARTESIAN_POINT ( 'NONE',  ( -71.75000000204838102, 80.81189881250001861, -10.69163855873949132 ) ) ;
#6507 = CIRCLE ( 'NONE', #4981, 1.500000000000001332 ) ;
#6508 = VECTOR ( 'NONE', #6879, 1000.000000000000000 ) ;
#6509 = ORIENTED_EDGE ( 'NONE', *, *, #3645, .F. ) ;
#6510 = CARTESIAN_POINT ( 'NONE',  ( 47.00000000000000000, 55.00000000000000000, 0.000000000000000000 ) ) ;
#6511 = CARTESIAN_POINT ( 'NONE',  ( -42.07074724807011989, 61.10209548959944215, -20.11061483308460751 ) ) ;
#6512 =( LENGTH_UNIT ( ) NAMED_UNIT ( * ) SI_UNIT ( .MILLI., .METRE. ) );
#6513 = CARTESIAN_POINT ( 'NONE',  ( -48.14429339001110009, 75.47411806927735256, -5.508782930744743567 ) ) ;
#6514 = ORIENTED_EDGE ( 'NONE', *, *, #2950, .T. ) ;
#6515 = CARTESIAN_POINT ( 'NONE',  ( -73.34375000204839523, 55.00000000000000000, -25.81189881249999729 ) ) ;
#6516 = CARTESIAN_POINT ( 'NONE',  ( -72.31250000409677625, 72.67766952966368876, 17.67766952966368521 ) ) ;
#6517 = CARTESIAN_POINT ( 'NONE',  ( -6.160267096003628318, 59.12214581854949103, -20.69010011304746044 ) ) ;
#6518 = AXIS2_PLACEMENT_3D ( 'NONE', #6291, #9923, #1830 ) ;
#6519 = VERTEX_POINT ( 'NONE', #10756 ) ;
#6520 = CARTESIAN_POINT ( 'NONE',  ( -55.30273887647248188, 69.12493077113425954, 15.58380738211564598 ) ) ;
#6521 = CARTESIAN_POINT ( 'NONE',  ( -54.88146047731135013, 73.03677976846768161, 10.81065700633557825 ) ) ;
#6522 = FACE_OUTER_BOUND ( 'NONE', #9943, .T. ) ;
#6523 = SURFACE_STYLE_FILL_AREA ( #10984 ) ;
#6524 = CARTESIAN_POINT ( 'NONE',  ( 36.99999999999999289, 55.00000000000000000, 0.000000000000000000 ) ) ;
#6525 = CARTESIAN_POINT ( 'NONE',  ( -75.31250000000007105, 72.67766952966361771, -17.67766952966361416 ) ) ;
#6526 = ORIENTED_EDGE ( 'NONE', *, *, #1881, .T. ) ;
#6527 = LINE ( 'NONE', #933, #6346 ) ;
#6528 = CARTESIAN_POINT ( 'NONE',  ( -18.23626112837376567, 55.01086945185167565, 0.005850176292158671722 ) ) ;
#6529 = CARTESIAN_POINT ( 'NONE',  ( -42.28847398866372487, 57.21383472543325155, -4.495207825519515588 ) ) ;
#6530 = CIRCLE ( 'NONE', #2690, 1.500000000000001332 ) ;
#6531 = DIRECTION ( 'NONE',  ( 0.000000000000000000, 0.000000000000000000, -1.000000000000000000 ) ) ;
#6532 = VECTOR ( 'NONE', #1723, 1000.000000000000000 ) ;
#6533 = DIRECTION ( 'NONE',  ( -0.000000000000000000, -1.000000000000000000, -0.000000000000000000 ) ) ;
#6534 = CARTESIAN_POINT ( 'NONE',  ( -0.4175868455413908609, 49.57342814860067648, -4.454705972034904704 ) ) ;
#6535 = ORIENTED_EDGE ( 'NONE', *, *, #7486, .T. ) ;
#6536 = CARTESIAN_POINT ( 'NONE',  ( 4.595919313165082620, 34.88938507153989832, -6.102095433906166377 ) ) ;
#6537 = DIRECTION ( 'NONE',  ( -1.000000000000000000, 0.000000000000000000, -0.000000000000000000 ) ) ;
#6538 = CIRCLE ( 'NONE', #8243, 27.53333900685068869 ) ;
#6539 = EDGE_CURVE ( 'NONE', #364, #3733, #5595, .T. ) ;
#6540 = CARTESIAN_POINT ( 'NONE',  ( -28.32521755090752791, 51.94774187383560360, 3.973893490808335205 ) ) ;
#6541 = CARTESIAN_POINT ( 'NONE',  ( -4.182066831946702479, 3.358985280702821985, -0.1739375980333739413 ) ) ;
#6542 = CARTESIAN_POINT ( 'NONE',  ( -71.44842626887532333, 72.99142816090481745, 20.46173487478911568 ) ) ;
#6543 = CARTESIAN_POINT ( 'NONE',  ( -79.43750000204838102, 65.69163855873948421, -25.81189881250000440 ) ) ;
#6544 = ORIENTED_EDGE ( 'NONE', *, *, #432, .F. ) ;
#6545 = CARTESIAN_POINT ( 'NONE',  ( -76.25000000204838102, 65.69163855873948421, -25.81189881250000440 ) ) ;
#6546 = AXIS2_PLACEMENT_3D ( 'NONE', #871, #2626, #10988 ) ;
#6547 = CIRCLE ( 'NONE', #2131, 3.000000000000000000 ) ;
#6548 = VERTEX_POINT ( 'NONE', #1658 ) ;
#6549 = CARTESIAN_POINT ( 'NONE',  ( 2.500000000000000000, 0.000000000000000000, -0.5394676594665810399 ) ) ;
#6550 = CARTESIAN_POINT ( 'NONE',  ( -53.41065706016718195, 65.82748300578383294, 8.886592616255020616 ) ) ;
#6551 = EDGE_CURVE ( 'NONE', #7792, #8673, #8430, .T. ) ;
#6552 = EDGE_CURVE ( 'NONE', #10858, #8154, #6711, .T. ) ;
#6553 = CARTESIAN_POINT ( 'NONE',  ( 0.000000000000000000, 0.000000000000000000, -0.3755037691048591086 ) ) ;
#6554 = CARTESIAN_POINT ( 'NONE',  ( -75.00000000000001421, 80.21963981261983179, 0.1224285101258584668 ) ) ;
#6555 = VECTOR ( 'NONE', #6962, 1000.000000000000000 ) ;
#6556 = DIRECTION ( 'NONE',  ( -1.000000000000000000, -0.000000000000000000, -0.000000000000000000 ) ) ;
#6557 = AXIS2_PLACEMENT_3D ( 'NONE', #6510, #10137, #6574 ) ;
#6558 = ORIENTED_EDGE ( 'NONE', *, *, #1321, .T. ) ;
#6559 = CARTESIAN_POINT ( 'NONE',  ( -71.99927362086853577, 76.65063509461015201, 12.50000000000143352 ) ) ;
#6560 = CARTESIAN_POINT ( 'NONE',  ( -72.12500000204840944, 29.18810118750000626, -10.69163855873949309 ) ) ;
#6561 = CARTESIAN_POINT ( 'NONE',  ( -78.00000000000001421, 63.48528137423857487, -8.485278002320759683 ) ) ;
#6562 = FACE_BOUND ( 'NONE', #9132, .T. ) ;
#6563 = CARTESIAN_POINT ( 'NONE',  ( 2.915746493136800677, 49.57776560221653028, -4.450368587613543703 ) ) ;
#6564 = PRODUCT_CONTEXT ( 'NONE', #4096, 'mechanical' ) ;
#6565 = CARTESIAN_POINT ( 'NONE',  ( -16.74007107453484622, 72.97142029985381839, -12.70283111168554235 ) ) ;
#6566 = CARTESIAN_POINT ( 'NONE',  ( -5.000000000000000000, 2.419979747126329794, -5.788163366729714099 ) ) ;
#6567 = EDGE_LOOP ( 'NONE', ( #3181, #2227, #2801, #7102 ) ) ;
#6568 = CARTESIAN_POINT ( 'NONE',  ( 36.99999999999999289, 55.00000000000000000, 0.000000000000000000 ) ) ;
#6569 = LINE ( 'NONE', #7343, #3456 ) ;
#6570 = ORIENTED_EDGE ( 'NONE', *, *, #3591, .F. ) ;
#6571 = ADVANCED_FACE ( 'NONE', ( #10217 ), #150, .F. ) ;
#6572 = CARTESIAN_POINT ( 'NONE',  ( -18.69730990872651333, 70.57397863033268948, 14.11552877426516339 ) ) ;
#6573 = CARTESIAN_POINT ( 'NONE',  ( -76.43750000204839523, 44.30836144126050158, -25.81189881249999374 ) ) ;
#6574 = DIRECTION ( 'NONE',  ( 0.000000000000000000, 1.000000000000000000, 0.000000000000000000 ) ) ;
#6575 = CARTESIAN_POINT ( 'NONE',  ( -7.070747353360942178, 68.33360022464046324, -16.24461469319379603 ) ) ;
#6576 = CARTESIAN_POINT ( 'NONE',  ( 47.00000000000000000, 55.00000000000000000, 0.000000000000000000 ) ) ;
#6577 = ORIENTED_EDGE ( 'NONE', *, *, #8564, .T. ) ;
#6578 = DIRECTION ( 'NONE',  ( 0.000000000000000000, 1.000000000000000000, 0.000000000000000000 ) ) ;
#6579 = CARTESIAN_POINT ( 'NONE',  ( -3.820070243736458426, 53.39331019270914425, -4.746214706174638920 ) ) ;
#6580 = CARTESIAN_POINT ( 'NONE',  ( -7.030643242133587378, 62.08114452727563304, -19.79025909736091648 ) ) ;
#6581 = ORIENTED_EDGE ( 'NONE', *, *, #9679, .T. ) ;
#6582 = CARTESIAN_POINT ( 'NONE',  ( -54.99627942256360313, 69.86586178386589552, 14.86494236827769200 ) ) ;
#6583 = CARTESIAN_POINT ( 'NONE',  ( -63.32723919479404628, 46.95276866351182576, 19.42062151208882170 ) ) ;
#6584 = CYLINDRICAL_SURFACE ( 'NONE', #6643, 1.499999999999999556 ) ;
#6585 = CARTESIAN_POINT ( 'NONE',  ( 47.00000000000000000, 55.00000000000000000, 0.000000000000000000 ) ) ;
#6586 = EDGE_CURVE ( 'NONE', #3987, #9278, #2921, .T. ) ;
#6587 = LINE ( 'NONE', #3037, #7089 ) ;
#6588 = DIRECTION ( 'NONE',  ( 0.000000000000000000, 1.000000000000000000, 0.000000000000000000 ) ) ;
#6589 = ORIENTED_EDGE ( 'NONE', *, *, #11249, .F. ) ;
#6590 = CARTESIAN_POINT ( 'NONE',  ( -79.34375000000002842, 65.35533905932737753, 24.99999999999999645 ) ) ;
#6591 = CARTESIAN_POINT ( 'NONE',  ( -56.75693999477515206, 54.99569681699411205, -0.004837550478154266538 ) ) ;
#6592 = CARTESIAN_POINT ( 'NONE',  ( -60.95549686576197956, 52.78924107303826219, 4.487718700620877854 ) ) ;
#6593 = EDGE_CURVE ( 'NONE', #10886, #11411, #6339, .T. ) ;
#6594 = LINE ( 'NONE', #4783, #4238 ) ;
#6595 = DIRECTION ( 'NONE',  ( 6.033820786006286457E-17, -1.000000000000000000, 0.000000000000000000 ) ) ;
#6596 = CARTESIAN_POINT ( 'NONE',  ( -67.53217105066197234, 42.78699024297431919, 7.034873537760521600 ) ) ;
#6597 = VERTEX_POINT ( 'NONE', #7541 ) ;
#6598 = CARTESIAN_POINT ( 'NONE',  ( 16.47760469315713294, 57.74566955740679930, 20.97627666568605420 ) ) ;
#6599 = AXIS2_PLACEMENT_3D ( 'NONE', #6349, #5621, #27 ) ;
#6600 = DIRECTION ( 'NONE',  ( 0.000000000000000000, 0.000000000000000000, 1.000000000000000000 ) ) ;
#6601 = EDGE_CURVE ( 'NONE', #6455, #6801, #5623, .T. ) ;
#6602 = DIRECTION ( 'NONE',  ( 0.000000000000000000, 0.000000000000000000, 1.000000000000000000 ) ) ;
#6603 = CARTESIAN_POINT ( 'NONE',  ( -79.34375000204839523, 55.00000000000000000, -25.81189881249999729 ) ) ;
#6604 = CARTESIAN_POINT ( 'NONE',  ( -72.40625000204838102, 29.18810118750000271, 4.741568889096522788E-15 ) ) ;
#6605 = CARTESIAN_POINT ( 'NONE',  ( -71.75000000204838102, 80.81189881250001861, -10.69163855873949132 ) ) ;
#6606 = ORIENTED_EDGE ( 'NONE', *, *, #1024, .T. ) ;
#6607 = CARTESIAN_POINT ( 'NONE',  ( -76.25000000409677625, 30.00000000000000355, 4.592425496802573578E-15 ) ) ;
#6608 = VERTEX_POINT ( 'NONE', #11163 ) ;
#6609 = CARTESIAN_POINT ( 'NONE',  ( 22.62790096952807772, 77.74555051095916269, -10.40404169996586958 ) ) ;
#6610 = CARTESIAN_POINT ( 'NONE',  ( -40.87813363220659113, 57.05701126625427122, -13.86937383821729064 ) ) ;
#6611 = DIRECTION ( 'NONE',  ( 0.000000000000000000, 0.000000000000000000, -1.000000000000000000 ) ) ;
#6612 = CARTESIAN_POINT ( 'NONE',  ( -75.00000000000004263, 60.52393795488850969, -25.20097221523710473 ) ) ;
#6613 = DIRECTION ( 'NONE',  ( -1.000000000000000000, -0.000000000000000000, -0.000000000000000000 ) ) ;
#6614 = VERTEX_POINT ( 'NONE', #5747 ) ;
#6615 = LINE ( 'NONE', #10189, #8984 ) ;
#6616 = CARTESIAN_POINT ( 'NONE',  ( -71.65625000409677625, 30.00000000000000355, -10.35533905932738108 ) ) ;
#6617 = DIRECTION ( 'NONE',  ( -1.000000000000000000, -0.000000000000000000, -0.000000000000000000 ) ) ;
#6618 = CARTESIAN_POINT ( 'NONE',  ( -78.50000000000000000, 55.00000000000000000, -24.99999999999999645 ) ) ;
#6619 = CARTESIAN_POINT ( 'NONE',  ( 12.44324801771031908, 50.71611971558893828, 5.579753105726120488 ) ) ;
#6620 = CIRCLE ( 'NONE', #7003, 1.500000000000001332 ) ;
#6621 = CARTESIAN_POINT ( 'NONE',  ( -5.009734977179735260, 65.88268349231633181, 19.12133901698799221 ) ) ;
#6622 = CARTESIAN_POINT ( 'NONE',  ( -78.00000000000001421, 59.24264068711927678, -5.742637315201482906 ) ) ;
#6623 = EDGE_CURVE ( 'NONE', #9124, #10918, #6709, .T. ) ;
#6624 = EDGE_LOOP ( 'NONE', ( #7634, #9749 ) ) ;
#6625 = DIRECTION ( 'NONE',  ( -1.000000000000000000, -0.000000000000000000, -0.000000000000000000 ) ) ;
#6626 = DIRECTION ( 'NONE',  ( 0.000000000000000000, -0.000000000000000000, 1.000000000000000000 ) ) ;
#6627 = EDGE_LOOP ( 'NONE', ( #11642, #6356, #1353, #2631 ) ) ;
#6628 = CARTESIAN_POINT ( 'NONE',  ( 22.18771278451687579, 76.01886845420673922, 2.750080521686579793 ) ) ;
#6629 = CARTESIAN_POINT ( 'NONE',  ( -78.78125000204839523, 73.25176868561975141, 18.25176868561974075 ) ) ;
#6630 = CIRCLE ( 'NONE', #9104, 1.500000000000001332 ) ;
#6631 = CARTESIAN_POINT ( 'NONE',  ( -76.34375000000005684, 65.35533905932732068, 24.99999999999990052 ) ) ;
#6632 = CARTESIAN_POINT ( 'NONE',  ( -53.45210586504737904, 71.88419113761085555, 12.52116934359859002 ) ) ;
#6633 = LINE ( 'NONE', #381, #11587 ) ;
#6634 = ORIENTED_EDGE ( 'NONE', *, *, #10514, .T. ) ;
#6635 = DIRECTION ( 'NONE',  ( -0.000000000000000000, -0.000000000000000000, 1.000000000000000000 ) ) ;
#6636 = LINE ( 'NONE', #141, #9166 ) ;
#6637 = CIRCLE ( 'NONE', #11777, 1.500000000000001332 ) ;
#6638 = ORIENTED_EDGE ( 'NONE', *, *, #4103, .F. ) ;
#6639 = CARTESIAN_POINT ( 'NONE',  ( -31.66281119664097332, 33.97723560729814096, 0.0005193846780039007571 ) ) ;
#6640 = CARTESIAN_POINT ( 'NONE',  ( -60.69833702282029009, 56.03208645306531110, 20.99415308669729541 ) ) ;
#6641 = SURFACE_SIDE_STYLE ('',( #1049 ) ) ;
#6642 = CARTESIAN_POINT ( 'NONE',  ( -76.06250000409679046, 37.32233047033631124, -17.67766952966368166 ) ) ;
#6643 = AXIS2_PLACEMENT_3D ( 'NONE', #4772, #7538, #7304 ) ;
#6644 = CARTESIAN_POINT ( 'NONE',  ( -15.87853224631106919, 59.96722547271372861, 0.6578075836705260526 ) ) ;
#6645 = CARTESIAN_POINT ( 'NONE',  ( -75.40625000409677625, 80.00000000000001421, 10.35533905932737397 ) ) ;
#6646 = ORIENTED_EDGE ( 'NONE', *, *, #149, .F. ) ;
#6647 = CARTESIAN_POINT ( 'NONE',  ( -75.21875000000000000, 80.00000000000001421, -10.35533905932737753 ) ) ;
#6648 = CARTESIAN_POINT ( 'NONE',  ( -78.00000000000002842, 50.75735931288069480, 11.22792543327563131 ) ) ;
#6649 = CARTESIAN_POINT ( 'NONE',  ( 47.00000000000000000, 55.00000000000000000, 0.000000000000000000 ) ) ;
#6650 = DIRECTION ( 'NONE',  ( 0.000000000000000000, 0.000000000000000000, 1.000000000000000000 ) ) ;
#6651 = AXIS2_PLACEMENT_3D ( 'NONE', #5754, #2928, #2752 ) ;
#6652 = CARTESIAN_POINT ( 'NONE',  ( -74.75000000409677625, 30.00000000000000355, 4.592425496802573578E-15 ) ) ;
#6653 = CARTESIAN_POINT ( 'NONE',  ( 6.776654365471205921, 48.89940868992559331, 3.518858988106267738 ) ) ;
#6654 = EDGE_LOOP ( 'NONE', ( #5284, #6438 ) ) ;
#6655 = CARTESIAN_POINT ( 'NONE',  ( 12.52240408941406535, 44.41801188983610871, 18.37272825892985040 ) ) ;
#6656 = CARTESIAN_POINT ( 'NONE',  ( -80.00000000000000000, 54.99999999999999289, -1.499996628082203021 ) ) ;
#6657 = CARTESIAN_POINT ( 'NONE',  ( -1.734723475976807094E-14, -5.773502691896260863, -0.4465819873852071575 ) ) ;
#6658 = CARTESIAN_POINT ( 'NONE',  ( -5.000000000000000000, 2.886751345948126879, -0.4465819873852047150 ) ) ;
#6659 = EDGE_CURVE ( 'NONE', #8886, #879, #176, .T. ) ;
#6660 = CARTESIAN_POINT ( 'NONE',  ( -6.624926763187422019, 66.86059616939517980, 22.01099344385859879 ) ) ;
#6661 = CARTESIAN_POINT ( 'NONE',  ( -78.40625000204839523, 36.74823131438026280, 18.25176868561974786 ) ) ;
#6662 = B_SPLINE_CURVE_WITH_KNOTS ( 'NONE', 3,
 ( #6106, #1712, #4637, #746, #11023, #4361, #8794, #2834, #6501, #10749, #10130, #5142, #8077, #7899, #3393, #4421, #9856, #11712, #3460, #5203, #6284, #6168, #7004, #573, #7067, #10626, #9739, #10691, #2615, #2503, #9799, #1593, #3512, #5261, #7181, #1649 ),
 .UNSPECIFIED., .F., .F.,
 ( 4, 2, 2, 2, 2, 2, 2, 2, 2, 2, 2, 2, 2, 2, 2, 2, 2, 4 ),
 ( 0.09712894785450570945, 0.09788736314146703754, 0.09864577842842835176, 0.1001626090023510079, 0.1016794395762736641, 0.1031962701501963064, 0.1047131007241189626, 0.1062299312980416049, 0.1077467618719642611, 0.1092635924458869034, 0.1107804230198095596, 0.1122972535937322158, 0.1138140841676548581, 0.1153309147415775143, 0.1168477453155001566, 0.1183645758894228128, 0.1198814064633454690, 0.1213982370372681113 ),
 .UNSPECIFIED. ) ;
#6663 = ORIENTED_EDGE ( 'NONE', *, *, #776, .T. ) ;
#6664 = EDGE_CURVE ( 'NONE', #9420, #9375, #9600, .T. ) ;
#6665 = AXIS2_PLACEMENT_3D ( 'NONE', #7695, #2959, #3136 ) ;
#6666 = CARTESIAN_POINT ( 'NONE',  ( -76.90625000409677625, 80.00000000000001421, 10.35533905932737397 ) ) ;
#6667 = ORIENTED_EDGE ( 'NONE', *, *, #5858, .T. ) ;
#6668 = CARTESIAN_POINT ( 'NONE',  ( 4.229223612318539161, 66.01664316016955070, -22.44374699675972451 ) ) ;
#6669 = STYLED_ITEM ( 'NONE', ( #8905 ), #7857 ) ;
#6670 = CARTESIAN_POINT ( 'NONE',  ( -40.58948485229369396, 56.37310121344063418, -13.95855491746121579 ) ) ;
#6671 = EDGE_CURVE ( 'NONE', #9881, #7673, #8772, .T. ) ;
#6672 = CARTESIAN_POINT ( 'NONE',  ( -75.00000000000000000, 55.00000000000000000, -25.00000000000000355 ) ) ;
#6673 = CARTESIAN_POINT ( 'NONE',  ( -75.00000000000002842, 69.01357686183018814, -21.46027625722670606 ) ) ;
#6674 = CYLINDRICAL_SURFACE ( 'NONE', #2640, 2.500000000000000000 ) ;
#6675 = VECTOR ( 'NONE', #5465, 1000.000000000000000 ) ;
#6676 = ORIENTED_EDGE ( 'NONE', *, *, #5956, .T. ) ;
#6677 = CARTESIAN_POINT ( 'NONE',  ( -74.00000000000000000, 55.00000000000000000, -24.99999999999999645 ) ) ;
#6678 = CARTESIAN_POINT ( 'NONE',  ( -74.75000000409677625, 30.00000000000000355, 4.592425496802573578E-15 ) ) ;
#6679 = DIRECTION ( 'NONE',  ( 0.000000000000000000, 0.8660255361751957315, 0.4999997706924120267 ) ) ;
#6680 = CARTESIAN_POINT ( 'NONE',  ( -24.10991423831773517, 51.46493228316985835, 6.139939154236729202 ) ) ;
#6681 = CARTESIAN_POINT ( 'NONE',  ( -73.06250000000008527, 37.32233047033641071, 17.67766952966358929 ) ) ;
#6682 = EDGE_CURVE ( 'NONE', #3451, #3280, #1176, .T. ) ;
#6683 = CARTESIAN_POINT ( 'NONE',  ( 2.500000000000000000, 0.000000000000000000, -4.860324802323723326 ) ) ;
#6684 = ORIENTED_EDGE ( 'NONE', *, *, #542, .F. ) ;
#6685 = LINE ( 'NONE', #10316, #9509 ) ;
#6686 = DIRECTION ( 'NONE',  ( 0.000000000000000000, 0.000000000000000000, 1.000000000000000000 ) ) ;
#6687 = ORIENTED_EDGE ( 'NONE', *, *, #3827, .F. ) ;
#6688 = CARTESIAN_POINT ( 'NONE',  ( -32.99614454614441428, 33.97685596767119165, 0.0005149883856687357403 ) ) ;
#6689 = CARTESIAN_POINT ( 'NONE',  ( -75.96875000204839523, 80.81189881250000440, -1.580522963032174394E-15 ) ) ;
#6690 = EDGE_CURVE ( 'NONE', #2686, #6077, #2142, .T. ) ;
#6691 = EDGE_CURVE ( 'NONE', #10318, #9906, #2856, .T. ) ;
#6692 = DIRECTION ( 'NONE',  ( -1.000000000000000000, -6.033820786006286457E-17, 0.000000000000000000 ) ) ;
#6693 = CARTESIAN_POINT ( 'NONE',  ( -79.43750000000004263, 72.67766952966367455, 17.67766952966366745 ) ) ;
#6694 = VECTOR ( 'NONE', #8438, 1000.000000000000000 ) ;
#6695 = DIRECTION ( 'NONE',  ( -1.000000000000000000, -0.000000000000000000, -0.000000000000000000 ) ) ;
#6696 = EDGE_LOOP ( 'NONE', ( #10050, #10340, #11791, #9995, #2567, #8898, #7779, #5843 ) ) ;
#6697 = CARTESIAN_POINT ( 'NONE',  ( -73.53125000204839523, 36.74823131438024859, -18.25176868561973720 ) ) ;
#6698 = ADVANCED_FACE ( 'NONE', ( #9260 ), #1052, .T. ) ;
#6699 = PLANE ( 'NONE',  #8604 ) ;
#6700 = CARTESIAN_POINT ( 'NONE',  ( 6.058385820703728442, 34.79737119409461599, 6.139092558150637480 ) ) ;
#6701 = ORIENTED_EDGE ( 'NONE', *, *, #11407, .T. ) ;
#6702 = CARTESIAN_POINT ( 'NONE',  ( 22.85428395102741206, 76.02051159816545578, 2.750403924439354775 ) ) ;
#6703 = AXIS2_PLACEMENT_3D ( 'NONE', #6524, #1953, #11771 ) ;
#6704 = CARTESIAN_POINT ( 'NONE',  ( 16.46050413285405511, 62.04246480880237158, 12.21692500290179417 ) ) ;
#6705 = DIRECTION ( 'NONE',  ( -1.000000000000000000, -0.000000000000000000, -0.000000000000000000 ) ) ;
#6706 = DIRECTION ( 'NONE',  ( -1.000000000000000000, -6.033820786006286457E-17, -0.000000000000000000 ) ) ;
#6707 = AXIS2_PLACEMENT_3D ( 'NONE', #3362, #2184, #5854 ) ;
#6708 = DIRECTION ( 'NONE',  ( -1.000000000000000000, -0.000000000000000000, -0.000000000000000000 ) ) ;
#6709 = LINE ( 'NONE', #10339, #7891 ) ;
#6710 = VERTEX_POINT ( 'NONE', #2478 ) ;
#6711 =( BOUNDED_CURVE ( )  B_SPLINE_CURVE ( 2, ( #3754, #3817, #333, #3880, #4842, #272, #11108 ),
 .UNSPECIFIED., .F., .T. ) 
 B_SPLINE_CURVE_WITH_KNOTS ( ( 3, 2, 2, 3 ),
 ( 0.7921800998908017366, 0.8119924382482776037, 0.8318047766057536929, 0.8449751200525960071 ),
 .UNSPECIFIED. ) 
 CURVE ( )  GEOMETRIC_REPRESENTATION_ITEM ( )  RATIONAL_B_SPLINE_CURVE ( ( 1.000000000000000000, 0.9238795325112867385, 1.000000000000000000, 0.9238795325112867385, 1.000000000000000000, 0.9493985947158180005, 0.9660721892104719988 ) ) 
 REPRESENTATION_ITEM ( '' )  );
#6712 = CARTESIAN_POINT ( 'NONE',  ( -78.59375000000001421, 44.64466094067260826, -24.99999999999998934 ) ) ;
#6713 = CARTESIAN_POINT ( 'NONE',  ( -78.00000000000001421, 50.75735931288069480, -2.742637315201482462 ) ) ;
#6714 = VECTOR ( 'NONE', #3197, 1000.000000000000000 ) ;
#6715 = CARTESIAN_POINT ( 'NONE',  ( -1.734723475976807094E-14, -5.773502691896260863, -5.653418012614792154 ) ) ;
#6716 = CARTESIAN_POINT ( 'NONE',  ( 19.22346612386121123, 61.13239903974351108, 3.531884177702926841 ) ) ;
#6717 = VERTEX_POINT ( 'NONE', #8834 ) ;
#6718 = CARTESIAN_POINT ( 'NONE',  ( -7.662811188708723797, 69.86483622371564195, -14.86557385339502169 ) ) ;
#6719 = DIRECTION ( 'NONE',  ( -1.000000000000000000, 0.000000000000000000, 0.000000000000000000 ) ) ;
#6720 = LINE ( 'NONE', #2149, #3332 ) ;
#6721 = ADVANCED_BREP_SHAPE_REPRESENTATION ( '', ( #4897, #4738 ), #10420 ) ;
#6722 = DIRECTION ( 'NONE',  ( 0.000000000000000000, 0.000000000000000000, -1.000000000000000000 ) ) ;
#6723 = CARTESIAN_POINT ( 'NONE',  ( -20.92478415792846036, 76.34167033271135949, 13.02563361730251223 ) ) ;
#6724 = CARTESIAN_POINT ( 'NONE',  ( -77.37500000204838102, 80.81189881250001861, 10.69163855873948599 ) ) ;
#6725 = CONICAL_SURFACE ( 'NONE', #8052, 17.04557674096337649, 0.1745329251994333364 ) ;
#6726 = VERTEX_POINT ( 'NONE', #11747 ) ;
#6727 = CARTESIAN_POINT ( 'NONE',  ( -73.06250000204840944, 80.81189881250001861, -10.69163855873949132 ) ) ;
#6728 = FACE_BOUND ( 'NONE', #2400, .T. ) ;
#6729 = CARTESIAN_POINT ( 'NONE',  ( 24.88384946230766559, 79.65201046289482179, -4.239228961464539758 ) ) ;
#6730 = CARTESIAN_POINT ( 'NONE',  ( -51.66851517836372665, 67.95242035046020135, 5.365460588887749793 ) ) ;
#6731 = VECTOR ( 'NONE', #4154, 1000.000000000000000 ) ;
#6732 = DIRECTION ( 'NONE',  ( 0.000000000000000000, 1.000000000000000000, 0.000000000000000000 ) ) ;
#6733 = DIRECTION ( 'NONE',  ( -6.033820786006286457E-17, 1.000000000000000000, 0.000000000000000000 ) ) ;
#6734 = CARTESIAN_POINT ( 'NONE',  ( 53.00000000000000000, 51.46446609406726935, -3.535533905932738197 ) ) ;
#6735 = ORIENTED_EDGE ( 'NONE', *, *, #9371, .T. ) ;
#6736 = AXIS2_PLACEMENT_3D ( 'NONE', #5716, #9353, #4812 ) ;
#6737 = CIRCLE ( 'NONE', #8642, 2.500000000000000000 ) ;
#6738 = CARTESIAN_POINT ( 'NONE',  ( -72.87500000000000000, 30.00000000000000355, 4.592425496802573578E-15 ) ) ;
#6739 = CARTESIAN_POINT ( 'NONE',  ( 0.000000000000000000, 0.000000000000000000, -6.099999999999999645 ) ) ;
#6740 = CARTESIAN_POINT ( 'NONE',  ( -37.65876738585033934, 51.02620280256623886, -3.052412481529861665 ) ) ;
#6741 = ORIENTED_EDGE ( 'NONE', *, *, #1072, .F. ) ;
#6742 = CARTESIAN_POINT ( 'NONE',  ( 3.500170968731791898, 49.14645465064588592, -3.907445888089149832 ) ) ;
#6743 = FACE_OUTER_BOUND ( 'NONE', #3067, .T. ) ;
#6744 = EDGE_CURVE ( 'NONE', #66, #1659, #5768, .T. ) ;
#6745 = AXIS2_PLACEMENT_3D ( 'NONE', #1000, #8260, #1836 ) ;
#6746 = DIRECTION ( 'NONE',  ( 0.000000000000000000, 1.000000000000000000, 0.000000000000000000 ) ) ;
#6747 = AXIS2_PLACEMENT_3D ( 'NONE', #8890, #1577, #10608 ) ;
#6748 = VERTEX_POINT ( 'NONE', #3371 ) ;
#6749 = FACE_OUTER_BOUND ( 'NONE', #181, .T. ) ;
#6750 = CARTESIAN_POINT ( 'NONE',  ( -77.28125000204838102, 55.00000000000000000, 25.81189881249999729 ) ) ;
#6751 = ORIENTED_EDGE ( 'NONE', *, *, #190, .T. ) ;
#6752 = CARTESIAN_POINT ( 'NONE',  ( -50.14429338685609849, 75.46958046783008456, -5.506903914760000518 ) ) ;
#6753 = CARTESIAN_POINT ( 'NONE',  ( -75.50000000204840944, 44.30836144126053000, 25.81189881250000795 ) ) ;
#6754 = FACE_BOUND ( 'NONE', #7352, .T. ) ;
#6755 = CARTESIAN_POINT ( 'NONE',  ( -52.00383529082647271, 74.42722782460430153, 8.047526119559261559 ) ) ;
#6756 =( NAMED_UNIT ( * ) PLANE_ANGLE_UNIT ( ) SI_UNIT ( $, .RADIAN. ) );
#6757 = CARTESIAN_POINT ( 'NONE',  ( -77.37500000409677625, 55.00000000000000000, -24.99999999999999645 ) ) ;
#6758 = ORIENTED_EDGE ( 'NONE', *, *, #4777, .T. ) ;
#6759 = CARTESIAN_POINT ( 'NONE',  ( -73.06250000204842365, 80.81189881250000440, -10.69163855873948954 ) ) ;
#6760 = EDGE_CURVE ( 'NONE', #89, #2384, #3318, .T. ) ;
#6761 = DIRECTION ( 'NONE',  ( 0.000000000000000000, -0.000000000000000000, -1.000000000000000000 ) ) ;
#6762 = CARTESIAN_POINT ( 'NONE',  ( -17.27494751259140315, 73.62640980466187557, 9.944421848179040069 ) ) ;
#6763 = ORIENTED_EDGE ( 'NONE', *, *, #3083, .T. ) ;
#6764 = CARTESIAN_POINT ( 'NONE',  ( -2.810961525112865012, 49.49246827230374635, -20.47109371692935298 ) ) ;
#6765 = CARTESIAN_POINT ( 'NONE',  ( -59.82750509709391196, 59.10995506582904824, 20.69284243654335498 ) ) ;
#6766 = CARTESIAN_POINT ( 'NONE',  ( -78.00000000000002842, 59.24264068711927678, 12.72792543327563131 ) ) ;
#6767 = LINE ( 'NONE', #1229, #3351 ) ;
#6768 = UNCERTAINTY_MEASURE_WITH_UNIT (LENGTH_MEASURE( 1.000000000000000082E-05 ), #11276, 'distance_accuracy_value', 'NONE');
#6769 = DIRECTION ( 'NONE',  ( 1.000000000000000000, 0.000000000000000000, -0.000000000000000000 ) ) ;
#6770 = EDGE_CURVE ( 'NONE', #11030, #9242, #123, .T. ) ;
#6771 = VERTEX_POINT ( 'NONE', #4459 ) ;
#6772 = CARTESIAN_POINT ( 'NONE',  ( -79.81250000000001421, 72.67766952966368876, -17.67766952966368876 ) ) ;
#6773 = CARTESIAN_POINT ( 'NONE',  ( -71.32904977408374236, 54.99618961743304624, -0.002957579938396712443 ) ) ;
#6774 = DIRECTION ( 'NONE',  ( 6.033820786006286457E-17, -1.000000000000000000, 0.000000000000000000 ) ) ;
#6775 = CARTESIAN_POINT ( 'NONE',  ( 16.89002048584296745, 59.31391198272093845, 5.609897141675635801 ) ) ;
#6776 = ORIENTED_EDGE ( 'NONE', *, *, #4299, .F. ) ;
#6777 = EDGE_CURVE ( 'NONE', #9231, #1770, #10607, .T. ) ;
#6778 = CARTESIAN_POINT ( 'NONE',  ( -22.47759590436300314, 52.25445647903773505, 21.02373912143526979 ) ) ;
#6779 = DIRECTION ( 'NONE',  ( -1.000000000000000000, -0.000000000000000000, -0.000000000000000000 ) ) ;
#6780 = CARTESIAN_POINT ( 'NONE',  ( -15.00000000000000000, -24.99999999999999645, -10.00000000000000000 ) ) ;
#6781 = CARTESIAN_POINT ( 'NONE',  ( -78.96875000204839523, 80.81189881250000440, -1.580522963032174394E-15 ) ) ;
#6782 = PLANE ( 'NONE',  #11449 ) ;
#6783 = CARTESIAN_POINT ( 'NONE',  ( -76.71875000204839523, 29.18810118750000271, 4.741568889096522788E-15 ) ) ;
#6784 = ORIENTED_EDGE ( 'NONE', *, *, #6156, .T. ) ;
#6785 = CARTESIAN_POINT ( 'NONE',  ( -73.53125000204839523, 36.74823131438024859, -18.25176868561973720 ) ) ;
#6786 = CARTESIAN_POINT ( 'NONE',  ( 47.00000000000000000, 50.00000000000000000, 0.000000000000000000 ) ) ;
#6787 = CARTESIAN_POINT ( 'NONE',  ( -64.86550693891295793, 42.79548891016047918, 7.031200541850135544 ) ) ;
#6788 = CARTESIAN_POINT ( 'NONE',  ( -78.31250000204838102, 29.18810118750000626, -10.69163855873949132 ) ) ;
#6789 = EDGE_CURVE ( 'NONE', #4962, #10562, #6087, .T. ) ;
#6790 = VECTOR ( 'NONE', #2621, 1000.000000000000000 ) ;
#6791 = DIRECTION ( 'NONE',  ( 1.000000000000000000, 0.000000000000000000, 0.000000000000000000 ) ) ;
#6792 = CYLINDRICAL_SURFACE ( 'NONE', #9140, 21.50000000000000000 ) ;
#6793 = ORIENTED_EDGE ( 'NONE', *, *, #4103, .T. ) ;
#6794 = CARTESIAN_POINT ( 'NONE',  ( -73.62500000000000000, 80.00000000000000000, -1.530808498934191324E-15 ) ) ;
#6795 = CARTESIAN_POINT ( 'NONE',  ( -74.37500000409677625, 55.00000000000000000, -24.99999999999999645 ) ) ;
#6796 = CARTESIAN_POINT ( 'NONE',  ( -52.03951664420899448, 59.99999999999998579, -0.3298728053696415308 ) ) ;
#6797 = VERTEX_POINT ( 'NONE', #7936 ) ;
#6798 = B_SPLINE_CURVE_WITH_KNOTS ( 'NONE', 3,
 ( #7984, #3424, #5288, #2713, #5409, #4568, #6199, #5350 ),
 .UNSPECIFIED., .F., .F.,
 ( 4, 2, 2, 4 ),
 ( 0.002921158011986708155, 0.003648658599403066180, 0.004376159186819424639, 0.005831160361652140689 ),
 .UNSPECIFIED. ) ;
#6799 = CARTESIAN_POINT ( 'NONE',  ( -18.66680221850326760, 57.68121094790071623, 6.472159763528865462 ) ) ;
#6800 = DIRECTION ( 'NONE',  ( 0.000000000000000000, 1.000000000000000000, 0.000000000000000000 ) ) ;
#6801 = VERTEX_POINT ( 'NONE', #3432 ) ;
#6802 = FACE_OUTER_BOUND ( 'NONE', #6271, .T. ) ;
#6803 = CARTESIAN_POINT ( 'NONE',  ( -78.21875000204839523, 36.74823131438024859, -18.25176868561973720 ) ) ;
#6804 = EDGE_LOOP ( 'NONE', ( #8234, #5549 ) ) ;
#6805 = CARTESIAN_POINT ( 'NONE',  ( -21.63602683877659771, 62.08561388645346568, 19.80191166437241179 ) ) ;
#6806 = CARTESIAN_POINT ( 'NONE',  ( -71.93750000204838102, 44.30836144126050158, -25.81189881249999374 ) ) ;
#6807 = AXIS2_PLACEMENT_3D ( 'NONE', #5127, #10790, #8892 ) ;
#6808 = CARTESIAN_POINT ( 'NONE',  ( -80.00000000000001421, 63.48528137423857487, -9.985278002320759683 ) ) ;
#6809 = CARTESIAN_POINT ( 'NONE',  ( -48.14429339001110009, 75.47411806927735256, -5.508782930744743567 ) ) ;
#6810 =( NAMED_UNIT ( * ) PLANE_ANGLE_UNIT ( ) SI_UNIT ( $, .RADIAN. ) );
#6811 = CARTESIAN_POINT ( 'NONE',  ( -78.00000000000001421, 63.48528137423857487, 9.985284746156350977 ) ) ;
#6812 = ORIENTED_EDGE ( 'NONE', *, *, #2586, .T. ) ;
#6813 = LINE ( 'NONE', #2423, #1293 ) ;
#6814 = EDGE_CURVE ( 'NONE', #6052, #388, #10731, .T. ) ;
#6815 = ADVANCED_FACE ( 'NONE', ( #5298 ), #8846, .T. ) ;
#6816 = DIRECTION ( 'NONE',  ( 0.000000000000000000, -1.000000000000000000, 0.000000000000000000 ) ) ;
#6817 = CARTESIAN_POINT ( 'NONE',  ( -26.81096152405270061, 44.41979049410412017, 18.36814973051028588 ) ) ;
#6818 = ORIENTED_EDGE ( 'NONE', *, *, #5169, .T. ) ;
#6819 = CARTESIAN_POINT ( 'NONE',  ( -8.996144538211344965, 69.86510777810948980, -14.86583919048846170 ) ) ;
#6820 = CARTESIAN_POINT ( 'NONE',  ( -42.36967124068387136, 54.31236102449236824, -13.99392387036892238 ) ) ;
#6821 = DIRECTION ( 'NONE',  ( 1.000000000000000000, 6.033820786006286457E-17, 0.000000000000000000 ) ) ;
#6822 = CARTESIAN_POINT ( 'NONE',  ( -76.62500000409677625, 55.00000000000000000, 24.99999999999999645 ) ) ;
#6823 = DIRECTION ( 'NONE',  ( 0.000000000000000000, 1.000000000000000000, 0.000000000000000000 ) ) ;
#6824 = ORIENTED_EDGE ( 'NONE', *, *, #5936, .T. ) ;
#6825 = CARTESIAN_POINT ( 'NONE',  ( -78.50000000000000000, 55.00000000000000000, -24.99999999999999645 ) ) ;
#6826 = DIRECTION ( 'NONE',  ( 0.000000000000000000, 1.000000000000000000, 0.000000000000000000 ) ) ;
#6827 = EDGE_CURVE ( 'NONE', #241, #7948, #3675, .T. ) ;
#6828 = CARTESIAN_POINT ( 'NONE',  ( -80.00000000000001421, 67.72792206135787296, -4.242637315201482906 ) ) ;
#6829 = AXIS2_PLACEMENT_3D ( 'NONE', #6576, #10206, #5980 ) ;
#6830 = EDGE_CURVE ( 'NONE', #9231, #10654, #4827, .T. ) ;
#6831 = EDGE_CURVE ( 'NONE', #4892, #9278, #2597, .T. ) ;
#6832 = CARTESIAN_POINT ( 'NONE',  ( 0.000000000000000000, 0.000000000000000000, -3.482085714285714229 ) ) ;
#6833 = CARTESIAN_POINT ( 'NONE',  ( -39.10991423111748588, 50.68603547566416978, -5.609840947021430324 ) ) ;
#6834 = ORIENTED_EDGE ( 'NONE', *, *, #9295, .F. ) ;
#6835 = CARTESIAN_POINT ( 'NONE',  ( -13.85565285731654761, 75.43037139504293975, 5.490367781071763709 ) ) ;
#6836 = DIRECTION ( 'NONE',  ( -1.000000000000000000, -0.000000000000000000, -0.000000000000000000 ) ) ;
#6837 = CARTESIAN_POINT ( 'NONE',  ( 0.000000000000000000, 0.000000000000000000, 0.000000000000000000 ) ) ;
#6838 = CARTESIAN_POINT ( 'NONE',  ( -76.34375000204839523, 55.00000000000000000, -25.81189881249999729 ) ) ;
#6839 = CARTESIAN_POINT ( 'NONE',  ( -75.87500000000007105, 30.00000000000010303, 4.592425496802555434E-15 ) ) ;
#6840 = CARTESIAN_POINT ( 'NONE',  ( -77.00000000204838102, 44.30836144126053000, 25.81189881250000795 ) ) ;
#6841 = EDGE_CURVE ( 'NONE', #10318, #7355, #3261, .T. ) ;
#6842 = EDGE_CURVE ( 'NONE', #9989, #9742, #6265, .T. ) ;
#6843 = EDGE_LOOP ( 'NONE', ( #2634, #2556 ) ) ;
#6844 = CARTESIAN_POINT ( 'NONE',  ( -74.09375000204839523, 55.00000000000000000, 25.81189881249999729 ) ) ;
#6845 = FACE_BOUND ( 'NONE', #2505, .T. ) ;
#6846 = CARTESIAN_POINT ( 'NONE',  ( 52.99999999999999289, 58.53553390593273065, 3.535533905932731091 ) ) ;
#6847 = EDGE_CURVE ( 'NONE', #11145, #7332, #9897, .T. ) ;
#6848 = CARTESIAN_POINT ( 'NONE',  ( 14.14423903981857755, 49.50929293985068114, 20.43023407247793699 ) ) ;
#6849 = AXIS2_PLACEMENT_3D ( 'NONE', #4090, #7040, #9656 ) ;
#6850 = CARTESIAN_POINT ( 'NONE',  ( 0.000000000000000000, 0.000000000000000000, -4.696360911962001339 ) ) ;
#6851 = DIRECTION ( 'NONE',  ( -0.000000000000000000, -0.000000000000000000, -1.000000000000000000 ) ) ;
#6852 = CARTESIAN_POINT ( 'NONE',  ( -73.25000000000000000, 55.00000000000000000, 24.99999999999999645 ) ) ;
#6853 = ORIENTED_EDGE ( 'NONE', *, *, #8771, .F. ) ;
#6854 = FACE_OUTER_BOUND ( 'NONE', #5100, .T. ) ;
#6855 = CIRCLE ( 'NONE', #11224, 5.249999999999998224 ) ;
#6856 = CARTESIAN_POINT ( 'NONE',  ( -73.25000000000000000, 55.00000000000000000, 24.99999999999999645 ) ) ;
#6857 = CARTESIAN_POINT ( 'NONE',  ( -73.81250000409677625, 72.67766952966368876, 17.67766952966368521 ) ) ;
#6858 = VECTOR ( 'NONE', #7436, 1000.000000000000114 ) ;
#6859 = CARTESIAN_POINT ( 'NONE',  ( -42.70536343102052257, 54.67063349880791634, -5.000011853200844847 ) ) ;
#6860 = ORIENTED_EDGE ( 'NONE', *, *, #382, .T. ) ;
#6861 = CARTESIAN_POINT ( 'NONE',  ( -51.04203483874748315, 61.59087299007505578, 2.357793790660874134 ) ) ;
#6862 = CARTESIAN_POINT ( 'NONE',  ( 0.000000000000000000, 0.000000000000000000, -5.560532340533429263 ) ) ;
#6863 = CARTESIAN_POINT ( 'NONE',  ( 39.99999999999999289, 55.00000000000000000, -5.249999999999998224 ) ) ;
#6864 = VERTEX_POINT ( 'NONE', #9007 ) ;
#6865 = CARTESIAN_POINT ( 'NONE',  ( 0.7329934142408522924, 64.99605696851787684, 19.59792961213366169 ) ) ;
#6866 = CARTESIAN_POINT ( 'NONE',  ( -79.06250000204839523, 80.81189881250000440, 10.69163855873948243 ) ) ;
#6867 = ORIENTED_EDGE ( 'NONE', *, *, #64, .F. ) ;
#6868 = CARTESIAN_POINT ( 'NONE',  ( -71.65625000204839523, 73.25176868561975141, -18.25176868561974430 ) ) ;
#6869 = AXIS2_PLACEMENT_3D ( 'NONE', #1977, #6556, #9348 ) ;
#6870 = DIRECTION ( 'NONE',  ( 0.000000000000000000, 1.000000000000000000, 0.000000000000000000 ) ) ;
#6871 = CARTESIAN_POINT ( 'NONE',  ( -64.47562408583945626, 38.19583575827792288, 12.92744520505189953 ) ) ;
#6872 = LINE ( 'NONE', #5734, #10250 ) ;
#6873 = VERTEX_POINT ( 'NONE', #8113 ) ;
#6874 = DIRECTION ( 'NONE',  ( -1.000000000000000000, -0.000000000000000000, -0.000000000000000000 ) ) ;
#6875 = CARTESIAN_POINT ( 'NONE',  ( -39.18898618735786243, 44.43394377878069434, -18.33326528472845141 ) ) ;
#6876 = ORIENTED_EDGE ( 'NONE', *, *, #5259, .T. ) ;
#6877 = CARTESIAN_POINT ( 'NONE',  ( -18.33720990162648690, 69.86853815246008992, 14.86915066445586042 ) ) ;
#6878 = CARTESIAN_POINT ( 'NONE',  ( -43.54480028671723346, 57.05700836894583716, -13.86810795104769412 ) ) ;
#6879 = DIRECTION ( 'NONE',  ( 0.8191520442889885789, 0.000000000000000000, 0.5735764363510507113 ) ) ;
#6880 = CARTESIAN_POINT ( 'NONE',  ( -80.00000000000001421, 59.24264068711928388, -11.22791868944003824 ) ) ;
#6881 = AXIS2_PLACEMENT_3D ( 'NONE', #11586, #10573, #4115 ) ;
#6882 = EDGE_LOOP ( 'NONE', ( #4471, #791 ) ) ;
#6883 = CARTESIAN_POINT ( 'NONE',  ( -76.62500000204839523, 44.30836144126050158, -25.81189881249999374 ) ) ;
#6884 = CARTESIAN_POINT ( 'NONE',  ( -75.00000000000001421, 51.71064787084756631, -25.65688961934584356 ) ) ;
#6885 = PRESENTATION_STYLE_ASSIGNMENT (( #8852 ) ) ;
#6886 =( GEOMETRIC_REPRESENTATION_CONTEXT ( 3 ) GLOBAL_UNCERTAINTY_ASSIGNED_CONTEXT ( ( #2870 ) ) GLOBAL_UNIT_ASSIGNED_CONTEXT ( ( #9951, #783, #10848 ) ) REPRESENTATION_CONTEXT ( 'NONE', 'WORKASPACE' ) );
#6887 = LINE ( 'NONE', #10515, #9318 ) ;
#6888 = CARTESIAN_POINT ( 'NONE',  ( -22.29127922628105551, 57.36276450979780606, 6.604096906534940636 ) ) ;
#6889 = VECTOR ( 'NONE', #8614, 1000.000000000000000 ) ;
#6890 = VERTEX_POINT ( 'NONE', #786 ) ;
#6891 = CARTESIAN_POINT ( 'NONE',  ( -52.00383529082647271, 74.42722782460430153, 8.047526119559261559 ) ) ;
#6892 = CARTESIAN_POINT ( 'NONE',  ( -78.00000000000002842, 54.99999999999998579, 8.485284746156354529 ) ) ;
#6893 = FACE_OUTER_BOUND ( 'NONE', #5864, .T. ) ;
#6894 = CARTESIAN_POINT ( 'NONE',  ( -75.59375000204839523, 55.00000000000000000, 25.81189881249999729 ) ) ;
#6895 = CARTESIAN_POINT ( 'NONE',  ( -12.39564893957180658, 69.98174787378947315, 20.04564381111873317 ) ) ;
#6896 = CARTESIAN_POINT ( 'NONE',  ( -75.03125000204839523, 36.74823131438024859, -18.25176868561973720 ) ) ;
#6897 = EDGE_LOOP ( 'NONE', ( #7706, #23, #3599, #209 ) ) ;
#6898 = CARTESIAN_POINT ( 'NONE',  ( -73.62500000409677625, 55.00000000000000000, 24.99999999999999645 ) ) ;
#6899 = DIRECTION ( 'NONE',  ( 0.000000000000000000, 0.000000000000000000, -1.000000000000000000 ) ) ;
#6900 = AXIS2_PLACEMENT_3D ( 'NONE', #8551, #7657, #332 ) ;
#6901 = EDGE_LOOP ( 'NONE', ( #10421, #3838, #6914, #6853, #500, #1377 ) ) ;
#6902 = AXIS2_PLACEMENT_3D ( 'NONE', #4483, #3519, #9863 ) ;
#6903 = CARTESIAN_POINT ( 'NONE',  ( -24.81096152833125856, 44.41791055217656492, 18.37268719335390443 ) ) ;
#6904 = CARTESIAN_POINT ( 'NONE',  ( -76.06250000204839523, 80.81189881250000440, 10.69163855873948243 ) ) ;
#6905 = DIRECTION ( 'NONE',  ( 0.000000000000000000, 0.000000000000000000, -1.000000000000000000 ) ) ;
#6906 = EDGE_CURVE ( 'NONE', #10565, #1970, #3552, .T. ) ;
#6907 = CARTESIAN_POINT ( 'NONE',  ( -78.00000000000000000, 55.00000000000000000, 0.000000000000000000 ) ) ;
#6908 = ORIENTED_EDGE ( 'NONE', *, *, #10668, .F. ) ;
#6909 = CARTESIAN_POINT ( 'NONE',  ( -79.34375000204839523, 55.00000000000000000, -25.81189881249999729 ) ) ;
#6910 = CARTESIAN_POINT ( 'NONE',  ( -77.46875000000000000, 30.00000000000001421, 10.35533905932739174 ) ) ;
#6911 = DIRECTION ( 'NONE',  ( -1.000000000000000000, -0.000000000000000000, -0.000000000000000000 ) ) ;
#6912 = DIRECTION ( 'NONE',  ( -1.000000000000000000, 0.000000000000000000, 0.000000000000000000 ) ) ;
#6913 = CIRCLE ( 'NONE', #8821, 1.500000000000001332 ) ;
#6914 = ORIENTED_EDGE ( 'NONE', *, *, #4700, .F. ) ;
#6915 = EDGE_CURVE ( 'NONE', #2813, #9256, #4038, .T. ) ;
#6916 = CARTESIAN_POINT ( 'NONE',  ( -63.77645048510821368, 49.38553753369352961, 4.319276899024868221 ) ) ;
#6917 = AXIS2_PLACEMENT_3D ( 'NONE', #9218, #3834, #6602 ) ;
#6918 = DIRECTION ( 'NONE',  ( 0.000000000000000000, 0.000000000000000000, 1.000000000000000000 ) ) ;
#6919 = SURFACE_SIDE_STYLE ('',( #7808 ) ) ;
#6920 = PRODUCT_DEFINITION_SHAPE ( 'NONE', 'NONE',  #3298 ) ;
#6921 = ORIENTED_EDGE ( 'NONE', *, *, #1181, .F. ) ;
#6922 = CARTESIAN_POINT ( 'NONE',  ( 4.665240958925800818, 65.77758632535075378, -19.17963262366009758 ) ) ;
#6923 = CONICAL_SURFACE ( 'NONE', #5011, 2.500000000000000000, 0.9599310885968755924 ) ;
#6924 = CIRCLE ( 'NONE', #1739, 27.53333900685068869 ) ;
#6925 = CARTESIAN_POINT ( 'NONE',  ( -77.00000000204839523, 29.18810118750000981, 10.69163855873950020 ) ) ;
#6926 = EDGE_LOOP ( 'NONE', ( #1131, #1060, #358, #11714 ) ) ;
#6927 = CARTESIAN_POINT ( 'NONE',  ( -73.62500000204842365, 29.18810118750000626, -10.69163855873949309 ) ) ;
#6928 = CARTESIAN_POINT ( 'NONE',  ( -75.59375000409677625, 80.00000000000001421, -10.35533905932737753 ) ) ;
#6929 = CARTESIAN_POINT ( 'NONE',  ( -15.00000000000000000, 5.000000000000000000, -20.00000000000000000 ) ) ;
#6930 = CARTESIAN_POINT ( 'NONE',  ( 8.496464703907626870, 55.00583224785918901, 0.0002657300979511648576 ) ) ;
#6931 = VECTOR ( 'NONE', #3479, 1000.000000000000000 ) ;
#6932 = CYLINDRICAL_SURFACE ( 'NONE', #1462, 2.500000000000000000 ) ;
#6933 = EDGE_LOOP ( 'NONE', ( #5809, #9630, #5903 ) ) ;
#6934 = CYLINDRICAL_SURFACE ( 'NONE', #517, 1.500000000000000000 ) ;
#6935 = ADVANCED_FACE ( 'NONE', ( #551 ), #4216, .F. ) ;
#6936 = CARTESIAN_POINT ( 'NONE',  ( -15.85565286160008469, 75.43490621471428881, 5.492246195135631837 ) ) ;
#6937 = ORIENTED_EDGE ( 'NONE', *, *, #11634, .T. ) ;
#6938 = CARTESIAN_POINT ( 'NONE',  ( 2.363972944155686928, 35.98715435331354939, -8.992005631236420271 ) ) ;
#6939 = CARTESIAN_POINT ( 'NONE',  ( -10.29698636593376371, 65.39011648954584643, -9.417152705430359205 ) ) ;
#6940 = VECTOR ( 'NONE', #4098, 1000.000000000000000 ) ;
#6941 = DIRECTION ( 'NONE',  ( 0.000000000000000000, -0.000000000000000000, 1.000000000000000000 ) ) ;
#6942 = CARTESIAN_POINT ( 'NONE',  ( -75.96875000409676204, 44.64466094067271484, -25.00000000000010303 ) ) ;
#6943 = CARTESIAN_POINT ( 'NONE',  ( -20.53797830674339764, 58.05056462116689175, 3.975025670360801566 ) ) ;
#6944 = ORIENTED_EDGE ( 'NONE', *, *, #11357, .F. ) ;
#6945 = CARTESIAN_POINT ( 'NONE',  ( -78.31250000204838102, 29.18810118750000626, -10.69163855873949309 ) ) ;
#6946 = CARTESIAN_POINT ( 'NONE',  ( -80.00000000000001421, 54.99999999999998579, -8.485278002320759683 ) ) ;
#6947 = DIRECTION ( 'NONE',  ( 0.000000000000000000, 1.000000000000000000, 0.000000000000000000 ) ) ;
#6948 = DIRECTION ( 'NONE',  ( -1.000000000000000000, -0.000000000000000000, -0.000000000000000000 ) ) ;
#6949 = CARTESIAN_POINT ( 'NONE',  ( -42.99986031074618609, 55.00026768892313100, -7.010501145347482144 ) ) ;
#6950 = ORIENTED_EDGE ( 'NONE', *, *, #6691, .T. ) ;
#6951 = CARTESIAN_POINT ( 'NONE',  ( -32.17314280228392676, 34.29902663375150240, -4.109485608336678197 ) ) ;
#6952 = EDGE_CURVE ( 'NONE', #4655, #9261, #8226, .T. ) ;
#6953 = CARTESIAN_POINT ( 'NONE',  ( 5.506399570602333426, 34.30736306936326230, 4.109392375493936100 ) ) ;
#6954 = CARTESIAN_POINT ( 'NONE',  ( 0.8192951148925836646, -5.300482436767290473, -0.1983443223721653714 ) ) ;
#6955 = CARTESIAN_POINT ( 'NONE',  ( -76.43750000204839523, 44.30836144126049447, -25.81189881249999019 ) ) ;
#6956 = DIRECTION ( 'NONE',  ( 0.000000000000000000, 1.000000000000000000, 0.000000000000000000 ) ) ;
#6957 = CARTESIAN_POINT ( 'NONE',  ( -76.06250000204840944, 80.81189881250001861, -10.69163855873949132 ) ) ;
#6958 = ORIENTED_EDGE ( 'NONE', *, *, #11325, .F. ) ;
#6959 = EDGE_CURVE ( 'NONE', #2643, #8769, #6913, .T. ) ;
#6960 = CARTESIAN_POINT ( 'NONE',  ( -75.50000000409677625, 80.00000000000000000, -1.530808498934191324E-15 ) ) ;
#6961 = CARTESIAN_POINT ( 'NONE',  ( 14.99999999999999645, 5.000000000000000000, 30.00000000000000711 ) ) ;
#6962 = DIRECTION ( 'NONE',  ( -0.000000000000000000, -1.000000000000000000, -0.000000000000000000 ) ) ;
#6963 = CARTESIAN_POINT ( 'NONE',  ( 6.329456780446692576, 33.97189653527247089, -0.0004287163746460355418 ) ) ;
#6964 = CARTESIAN_POINT ( 'NONE',  ( -76.81250000204838102, 29.18810118750000626, -10.69163855873949132 ) ) ;
#6965 = LINE ( 'NONE', #5887, #7228 ) ;
#6966 = ADVANCED_FACE ( 'NONE', ( #10064 ), #10908, .F. ) ;
#6967 = DIRECTION ( 'NONE',  ( 0.000000000000000000, 0.000000000000000000, -1.000000000000000000 ) ) ;
#6968 = ORIENTED_EDGE ( 'NONE', *, *, #2201, .F. ) ;
#6969 = DIRECTION ( 'NONE',  ( -1.000000000000000000, -0.000000000000000000, -0.000000000000000000 ) ) ;
#6970 = CARTESIAN_POINT ( 'NONE',  ( -73.53125000000000000, 80.00000000000001421, 10.35533905932737397 ) ) ;
#6971 = CARTESIAN_POINT ( 'NONE',  ( -68.74447550303376886, 50.00000002723004400, -0.0005274282990175871997 ) ) ;
#6972 = ORIENTED_EDGE ( 'NONE', *, *, #960, .T. ) ;
#6973 = DIRECTION ( 'NONE',  ( 0.000000000000000000, 0.000000000000000000, 1.000000000000000000 ) ) ;
#6974 = ORIENTED_EDGE ( 'NONE', *, *, #7835, .F. ) ;
#6975 = CARTESIAN_POINT ( 'NONE',  ( -31.49982903124580602, 48.09671445454723937, -1.369954454670364807 ) ) ;
#6976 = FACE_BOUND ( 'NONE', #3507, .T. ) ;
#6977 = CARTESIAN_POINT ( 'NONE',  ( 62.44550000000000267, 55.00000000000000000, 0.000000000000000000 ) ) ;
#6978 = ADVANCED_FACE ( 'NONE', ( #6380 ), #9177, .T. ) ;
#6979 = ADVANCED_FACE ( 'NONE', ( #5470 ), #4572, .F. ) ;
#6980 = CARTESIAN_POINT ( 'NONE',  ( 5.013139816730369347, 65.88383839924598817, 19.12068691178585311 ) ) ;
#6981 = CARTESIAN_POINT ( 'NONE',  ( -77.75000000204839523, 80.81189881250000440, -10.69163855873948954 ) ) ;
#6982 = ORIENTED_EDGE ( 'NONE', *, *, #111, .T. ) ;
#6983 = CIRCLE ( 'NONE', #6026, 1.500000000000001332 ) ;
#6984 = CARTESIAN_POINT ( 'NONE',  ( -77.84375000204839523, 55.00000000000000000, -25.81189881249999729 ) ) ;
#6985 = CARTESIAN_POINT ( 'NONE',  ( -78.00000000000002842, 54.99999999999998579, 6.985284746156355418 ) ) ;
#6986 = CARTESIAN_POINT ( 'NONE',  ( 0.000000000000000000, 0.000000000000000000, -0.02539999999999996774 ) ) ;
#6987 = FACE_OUTER_BOUND ( 'NONE', #4160, .T. ) ;
#6988 = DIRECTION ( 'NONE',  ( -1.000000000000000000, -0.000000000000000000, -0.000000000000000000 ) ) ;
#6989 = EDGE_CURVE ( 'NONE', #10642, #11523, #9117, .T. ) ;
#6990 = ORIENTED_EDGE ( 'NONE', *, *, #7785, .F. ) ;
#6991 = DIRECTION ( 'NONE',  ( 0.000000000000000000, 1.000000000000000000, 0.000000000000000000 ) ) ;
#6992 = CARTESIAN_POINT ( 'NONE',  ( -53.69727390230763575, 74.79022971164903311, 7.081167078663678893 ) ) ;
#6993 = EDGE_LOOP ( 'NONE', ( #4007, #9657, #5824, #10969 ) ) ;
#6994 = CARTESIAN_POINT ( 'NONE',  ( -26.85565286017724418, 42.10688304539454663, 16.77644304551772336 ) ) ;
#6995 = CARTESIAN_POINT ( 'NONE',  ( 0.4968476615399680107, 43.29813335323204626, -7.812534750456064714 ) ) ;
#6996 = CARTESIAN_POINT ( 'NONE',  ( -78.21875000204839523, 36.74823131438024859, -18.25176868561973720 ) ) ;
#6997 = AXIS2_PLACEMENT_3D ( 'NONE', #11698, #3499, #5245 ) ;
#6998 = ORIENTED_EDGE ( 'NONE', *, *, #3208, .T. ) ;
#6999 = CARTESIAN_POINT ( 'NONE',  ( -73.15625000000000000, 44.64466094067262958, 25.00000000000001066 ) ) ;
#7000 = CARTESIAN_POINT ( 'NONE',  ( -80.00000000000001421, 42.27207793864211283, -12.72791868944003824 ) ) ;
#7001 = EDGE_LOOP ( 'NONE', ( #3440, #7476 ) ) ;
#7003 = AXIS2_PLACEMENT_3D ( 'NONE', #7160, #11690, #3212 ) ;
#7002 = DIRECTION ( 'NONE',  ( 0.000000000000000000, 0.000000000000000000, -1.000000000000000000 ) ) ;
#7004 = CARTESIAN_POINT ( 'NONE',  ( 18.37142430252887237, 56.60669449543473775, 4.746147407754762071 ) ) ;
#7005 = CARTESIAN_POINT ( 'NONE',  ( -55.54150741847631423, 61.01381665909754304, 3.604391452501248150 ) ) ;
#7006 = ORIENTED_EDGE ( 'NONE', *, *, #776, .F. ) ;
#7007 = CARTESIAN_POINT ( 'NONE',  ( -50.27495406422890767, 76.01781437481966464, 2.059423474151367728 ) ) ;
#7008 = CARTESIAN_POINT ( 'NONE',  ( 17.52230480588388417, 67.92092721363508190, 16.80419350660125843 ) ) ;
#7009 = CARTESIAN_POINT ( 'NONE',  ( 37.00000000000000000, 50.00000000000000000, 0.000000000000000000 ) ) ;
#7010 = CARTESIAN_POINT ( 'NONE',  ( 0.000000000000000000, 0.000000000000000000, 0.000000000000000000 ) ) ;
#7011 = APPLICATION_CONTEXT ( 'automotive_design' ) ;
#7012 = CARTESIAN_POINT ( 'NONE',  ( -71.93750000204838102, 44.30836144126050158, -25.81189881249999374 ) ) ;
#7013 = VERTEX_POINT ( 'NONE', #8166 ) ;
#7014 = LINE ( 'NONE', #10637, #9958 ) ;
#7015 = DIRECTION ( 'NONE',  ( 0.000000000000000000, 0.000000000000000000, -1.000000000000000000 ) ) ;
#7016 = CARTESIAN_POINT ( 'NONE',  ( -72.03125000409679046, 44.64466094067237378, 24.99999999999975131 ) ) ;
#7017 = VECTOR ( 'NONE', #1298, 1000.000000000000114 ) ;
#7018 = CARTESIAN_POINT ( 'NONE',  ( -7.662811188708723797, 69.86483622371564195, -14.86557385339502169 ) ) ;
#7019 = EDGE_LOOP ( 'NONE', ( #10570, #9497, #11244, #1330 ) ) ;
#7020 = CARTESIAN_POINT ( 'NONE',  ( -76.71875000204839523, 36.74823131438024859, -18.25176868561973720 ) ) ;
#7021 = CIRCLE ( 'NONE', #5293, 5.249999999999998224 ) ;
#7022 = CARTESIAN_POINT ( 'NONE',  ( -71.09399662003431786, 50.00000004634800632, -0.0006807936302138478625 ) ) ;
#7023 = EDGE_CURVE ( 'NONE', #8687, #9261, #7335, .T. ) ;
#7024 = CARTESIAN_POINT ( 'NONE',  ( -80.00000000000001421, 59.24264068711928388, -12.72791868944003824 ) ) ;
#7025 = CARTESIAN_POINT ( 'NONE',  ( -44.96936008568403764, 63.99178041037959019, -19.01235157881157178 ) ) ;
#7026 = CIRCLE ( 'NONE', #10058, 1.500000000000001332 ) ;
#7027 = DIRECTION ( 'NONE',  ( -1.000000000000000000, -0.000000000000000000, -0.000000000000000000 ) ) ;
#7028 = CARTESIAN_POINT ( 'NONE',  ( -77.75000000204839523, 80.81189881250001861, -10.69163855873949132 ) ) ;
#7029 = DIRECTION ( 'NONE',  ( -1.000000000000000000, -0.000000000000000000, -0.000000000000000000 ) ) ;
#7030 = ORIENTED_EDGE ( 'NONE', *, *, #10177, .T. ) ;
#7031 = VECTOR ( 'NONE', #4453, 1000.000000000000000 ) ;
#7032 = CYLINDRICAL_SURFACE ( 'NONE', #11297, 1.500000000000000444 ) ;
#7033 = PRODUCT_DEFINITION_CONTEXT ( 'detailed design', #20, 'design' ) ;
#7034 = EDGE_LOOP ( 'NONE', ( #4396, #9555, #6387, #10015, #8015, #4384 ) ) ;
#7035 = ADVANCED_FACE ( 'NONE', ( #4630 ), #2722, .T. ) ;
#7036 = CARTESIAN_POINT ( 'NONE',  ( -47.44324763638165621, 61.84126198528888096, -1.841921628722773097 ) ) ;
#7037 = DIRECTION ( 'NONE',  ( -1.000000000000000000, -0.000000000000000000, -0.000000000000000000 ) ) ;
#7038 = ADVANCED_FACE ( 'NONE', ( #5650 ), #10245, .F. ) ;
#7039 = CARTESIAN_POINT ( 'NONE',  ( -0.4079457818577095773, 5.537975084925940372, -0.3106000600989312077 ) ) ;
#7040 = DIRECTION ( 'NONE',  ( 1.000000000000000000, 6.033820786006286457E-17, 0.000000000000000000 ) ) ;
#7041 = CARTESIAN_POINT ( 'NONE',  ( 8.874488085748957644, 67.64441578773138986, -18.00748785805702212 ) ) ;
#7042 = AXIS2_PLACEMENT_3D ( 'NONE', #9422, #9482, #10197 ) ;
#7043 = CARTESIAN_POINT ( 'NONE',  ( -75.12500000204838102, 44.30836144126049447, -25.81189881249999019 ) ) ;
#7044 = CIRCLE ( 'NONE', #4726, 1.500000000000001332 ) ;
#7045 = ORIENTED_EDGE ( 'NONE', *, *, #10885, .T. ) ;
#7046 = CARTESIAN_POINT ( 'NONE',  ( -76.15625000204839523, 73.25176868561975141, -18.25176868561974430 ) ) ;
#7047 = CARTESIAN_POINT ( 'NONE',  ( -5.000000000000000888, 0.9828435001097601820, -0.04309034703445699388 ) ) ;
#7048 = DIRECTION ( 'NONE',  ( -1.000000000000000000, 0.000000000000000000, 0.000000000000000000 ) ) ;
#7049 = CARTESIAN_POINT ( 'NONE',  ( 4.714426611521913557, 54.99241905126812924, -0.004073598914535226517 ) ) ;
#7050 = AXIS2_PLACEMENT_3D ( 'NONE', #4569, #8160, #4392 ) ;
#7051 = AXIS2_PLACEMENT_3D ( 'NONE', #1973, #11129, #294 ) ;
#7052 = DIRECTION ( 'NONE',  ( 0.000000000000000000, 0.000000000000000000, 1.000000000000000000 ) ) ;
#7053 = ORIENTED_EDGE ( 'NONE', *, *, #5790, .F. ) ;
#7054 = CARTESIAN_POINT ( 'NONE',  ( -27.51876704757110303, 50.51322248963012385, 2.212644460676499669 ) ) ;
#7055 = EDGE_CURVE ( 'NONE', #11654, #6519, #3465, .T. ) ;
#7056 = DIRECTION ( 'NONE',  ( 0.000000000000000000, 1.000000000000000000, 0.000000000000000000 ) ) ;
#7057 = ORIENTED_EDGE ( 'NONE', *, *, #8583, .T. ) ;
#7058 = CARTESIAN_POINT ( 'NONE',  ( -38.52231951926622600, 44.43456989975021543, -18.33175367071157780 ) ) ;
#7059 = CARTESIAN_POINT ( 'NONE',  ( -33.33147340253317736, 40.98517796169446825, 0.0004158008307579650481 ) ) ;
#7060 = CARTESIAN_POINT ( 'NONE',  ( -79.53125000204838102, 55.00000000000000000, -25.81189881249999729 ) ) ;
#7061 = ORIENTED_EDGE ( 'NONE', *, *, #7133, .F. ) ;
#7062 = CARTESIAN_POINT ( 'NONE',  ( -79.06250000204839523, 80.81189881250001861, 10.69163855873948599 ) ) ;
#7063 = CARTESIAN_POINT ( 'NONE',  ( 63.00000000000000000, 55.00000000000000000, 0.000000000000000000 ) ) ;
#7064 = FILL_AREA_STYLE_COLOUR ( '', #7996 ) ;
#7065 = EDGE_CURVE ( 'NONE', #10744, #5423, #2507, .T. ) ;
#7066 = DIRECTION ( 'NONE',  ( -1.000000000000000000, 0.000000000000000000, 0.000000000000000000 ) ) ;
#7067 = CARTESIAN_POINT ( 'NONE',  ( 19.52954336140098235, 57.50311058138565556, 4.340816333004676508 ) ) ;
#7068 = CARTESIAN_POINT ( 'NONE',  ( -33.66680225892029910, 47.99349995571937910, 0.0003166132758461101537 ) ) ;
#7069 = ORIENTED_EDGE ( 'NONE', *, *, #4687, .T. ) ;
#7070 = CARTESIAN_POINT ( 'NONE',  ( -6.003876560668130580, 63.04743182124521184, -19.42709301306817693 ) ) ;
#7071 = CARTESIAN_POINT ( 'NONE',  ( -78.00000000000002842, 54.99999999999998579, 9.985284746156354529 ) ) ;
#7072 = DIRECTION ( 'NONE',  ( 1.000000000000000000, 0.000000000000000000, 0.000000000000000000 ) ) ;
#7073 = CIRCLE ( 'NONE', #9546, 3.000000000000000888 ) ;
#7074 = CARTESIAN_POINT ( 'NONE',  ( 63.00000000000000000, 55.00000000000000000, -2.445500000000003116 ) ) ;
#7075 = CARTESIAN_POINT ( 'NONE',  ( -71.56250000204838102, 80.81189881250001861, -10.69163855873949132 ) ) ;
#7076 = ORIENTED_EDGE ( 'NONE', *, *, #7774, .T. ) ;
#7077 = CARTESIAN_POINT ( 'NONE',  ( 14.99999999999999645, 0.000000000000000000, -10.00000000000000000 ) ) ;
#7078 = DIRECTION ( 'NONE',  ( 0.000000000000000000, 1.000000000000000000, 0.000000000000000000 ) ) ;
#7079 = FACE_BOUND ( 'NONE', #4036, .T. ) ;
#7080 = CARTESIAN_POINT ( 'NONE',  ( 3.697305843545918513, 35.98616635274733255, -8.992456113074794644 ) ) ;
#7081 = AXIS2_PLACEMENT_3D ( 'NONE', #8133, #9922, #6113 ) ;
#7082 = EDGE_LOOP ( 'NONE', ( #2068, #3315, #7530, #4831, #6535, #4376, #2942, #7069, #2519, #8843, #4616, #5832 ) ) ;
#7083 = CARTESIAN_POINT ( 'NONE',  ( -75.01598058408755776, 56.74138771028714956, -25.81189881249999729 ) ) ;
#7084 = AXIS2_PLACEMENT_3D ( 'NONE', #1724, #700, #4486 ) ;
#7085 = DIRECTION ( 'NONE',  ( 1.000000000000000000, 0.000000000000000000, 0.000000000000000000 ) ) ;
#7086 = CARTESIAN_POINT ( 'NONE',  ( 36.99999999999999289, 55.00000000000000000, 0.000000000000000000 ) ) ;
#7087 = CARTESIAN_POINT ( 'NONE',  ( -54.59603348275399526, 73.54984634329692028, 9.912388241271610667 ) ) ;
#7088 = LINE ( 'NONE', #10539, #7512 ) ;
#7089 = VECTOR ( 'NONE', #5863, 1000.000000000000000 ) ;
#7090 = CARTESIAN_POINT ( 'NONE',  ( -76.71875000204839523, 36.74823131438024859, -18.25176868561973720 ) ) ;
#7091 = CARTESIAN_POINT ( 'NONE',  ( -78.00000000000001421, 63.48528137423857487, 1.500003371917795425 ) ) ;
#7092 = VECTOR ( 'NONE', #5905, 1000.000000000000000 ) ;
#7093 = VERTEX_POINT ( 'NONE', #964 ) ;
#7094 = DIRECTION ( 'NONE',  ( 0.000000000000000000, 0.000000000000000000, -1.000000000000000000 ) ) ;
#7095 = ORIENTED_EDGE ( 'NONE', *, *, #8813, .T. ) ;
#7096 = CARTESIAN_POINT ( 'NONE',  ( -28.87484158014380853, 48.19745421759348858, 1.704321637862361349 ) ) ;
#7097 = CARTESIAN_POINT ( 'NONE',  ( 8.673617379884035472E-16, 5.773502691896260863, -6.099999999999999645 ) ) ;
#7098 = CARTESIAN_POINT ( 'NONE',  ( -15.00000000000000355, 5.000000000000000000, 20.00000000000000000 ) ) ;
#7099 = VECTOR ( 'NONE', #10092, 1000.000000000000000 ) ;
#7100 = LINE ( 'NONE', #5410, #4937 ) ;
#7101 = CARTESIAN_POINT ( 'NONE',  ( -15.00000000000000000, -30.00000000000000000, 10.00000000000000000 ) ) ;
#7102 = ORIENTED_EDGE ( 'NONE', *, *, #3891, .T. ) ;
#7103 = CARTESIAN_POINT ( 'NONE',  ( -79.25000000204838102, 65.69163855873948421, -25.81189881250000440 ) ) ;
#7104 = CARTESIAN_POINT ( 'NONE',  ( -80.00000000000001421, 63.48528137423857487, -8.485278002320759683 ) ) ;
#7105 = CIRCLE ( 'NONE', #8060, 1.500000000000001332 ) ;
#7106 = ADVANCED_FACE ( 'NONE', ( #7388 ), #11015, .F. ) ;
#7107 = CARTESIAN_POINT ( 'NONE',  ( -77.00000000409677625, 80.00000000000000000, -1.530808498934191324E-15 ) ) ;
#7108 = CARTESIAN_POINT ( 'NONE',  ( 5.871464932984317819, 55.00507431483917031, 0.002345699056559674180 ) ) ;
#7109 = CARTESIAN_POINT ( 'NONE',  ( 47.00000000000000000, 58.53553390593273065, -3.535533905932743526 ) ) ;
#7110 = AXIS2_PLACEMENT_3D ( 'NONE', #7454, #2827, #10123 ) ;
#7111 = EDGE_LOOP ( 'NONE', ( #274, #1567 ) ) ;
#7112 = DIRECTION ( 'NONE',  ( -0.000000000000000000, -0.000000000000000000, -1.000000000000000000 ) ) ;
#7113 = AXIS2_PLACEMENT_3D ( 'NONE', #4394, #4455, #11303 ) ;
#7114 = DIRECTION ( 'NONE',  ( -1.000000000000000000, -0.000000000000000000, -0.000000000000000000 ) ) ;
#7115 = ORIENTED_EDGE ( 'NONE', *, *, #7197, .F. ) ;
#7116 = CARTESIAN_POINT ( 'NONE',  ( -42.26269064503769357, 57.05915346985771208, -20.93174897424885472 ) ) ;
#7117 = CARTESIAN_POINT ( 'NONE',  ( -46.16981911518406179, 62.81253473440293078, -11.70186679652239725 ) ) ;
#7118 = CARTESIAN_POINT ( 'NONE',  ( -76.34375000204839523, 73.25176868561975141, -18.25176868561974430 ) ) ;
#7119 = AXIS2_PLACEMENT_3D ( 'NONE', #7211, #2464, #6132 ) ;
#7120 = AXIS2_PLACEMENT_3D ( 'NONE', #6382, #6329, #11750 ) ;
#7121 = VERTEX_POINT ( 'NONE', #1924 ) ;
#7122 = CARTESIAN_POINT ( 'NONE',  ( -77.46875000204839523, 73.25176868561975141, 18.25176868561974075 ) ) ;
#7123 = DIRECTION ( 'NONE',  ( -1.000000000000000000, -0.000000000000000000, -0.000000000000000000 ) ) ;
#7124 =( NAMED_UNIT ( * ) SI_UNIT ( $, .STERADIAN. ) SOLID_ANGLE_UNIT ( ) );
#7125 = EDGE_CURVE ( 'NONE', #7495, #10833, #5597, .T. ) ;
#7126 = CARTESIAN_POINT ( 'NONE',  ( 19.99999999999996803, -63.00000000000000000, 5.000000000000000000 ) ) ;
#7127 = DIRECTION ( 'NONE',  ( -1.000000000000000000, 0.000000000000000000, 0.000000000000000000 ) ) ;
#7128 = CARTESIAN_POINT ( 'NONE',  ( 0.7144279133528070869, 54.99538305296515261, -0.002722153396144796379 ) ) ;
#7129 = ORIENTED_EDGE ( 'NONE', *, *, #733, .F. ) ;
#7130 = CARTESIAN_POINT ( 'NONE',  ( -68.34104732181945963, 33.99448141944315438, 0.006743540747239065887 ) ) ;
#7131 = CARTESIAN_POINT ( 'NONE',  ( -17.82693376281896391, 72.53768310958322729, 11.72612467905221934 ) ) ;
#7132 = CARTESIAN_POINT ( 'NONE',  ( -78.00000000000001421, 54.99999999999999289, -16.97055937655931501 ) ) ;
#7133 = EDGE_CURVE ( 'NONE', #10196, #2759, #835, .T. ) ;
#7134 = FACE_OUTER_BOUND ( 'NONE', #4017, .T. ) ;
#7135 = CARTESIAN_POINT ( 'NONE',  ( -78.00000000000001421, 67.72792206135787296, 5.742644059037073312 ) ) ;
#7136 = ORIENTED_EDGE ( 'NONE', *, *, #8112, .T. ) ;
#7137 = CARTESIAN_POINT ( 'NONE',  ( -72.50000000409677625, 80.00000000000000000, -1.530808498934191324E-15 ) ) ;
#7138 = FACE_OUTER_BOUND ( 'NONE', #10773, .T. ) ;
#7139 = FACE_BOUND ( 'NONE', #1702, .T. ) ;
#7140 = CARTESIAN_POINT ( 'NONE',  ( -31.30269415623623885, 33.99224428815358579, -1.031667027462585207 ) ) ;
#7141 = EDGE_LOOP ( 'NONE', ( #11818, #8452, #7956, #5307 ) ) ;
#7142 = PLANE ( 'NONE',  #8258 ) ;
#7143 = ADVANCED_FACE ( 'NONE', ( #3129 ), #10370, .F. ) ;
#7144 = CARTESIAN_POINT ( 'NONE',  ( -78.68750000409679046, 72.67766952966368876, -17.67766952966368876 ) ) ;
#7145 = VERTEX_POINT ( 'NONE', #8588 ) ;
#7146 = CARTESIAN_POINT ( 'NONE',  ( -83.00000000000000000, 55.00000000000000000, 0.000000000000000000 ) ) ;
#7147 = CARTESIAN_POINT ( 'NONE',  ( 16.79625880786201719, 58.05269072103210704, 3.973457567300640036 ) ) ;
#7148 = CARTESIAN_POINT ( 'NONE',  ( -71.99927368942448425, 76.65063862282433149, 12.49999388895319363 ) ) ;
#7149 = CARTESIAN_POINT ( 'NONE',  ( 36.99999999999999289, 55.00000000000000000, 0.000000000000000000 ) ) ;
#7150 = ORIENTED_EDGE ( 'NONE', *, *, #668, .F. ) ;
#7151 = CARTESIAN_POINT ( 'NONE',  ( 0.000000000000000000, 5.773502691896260863, -0.4465819873852071575 ) ) ;
#7152 = VERTEX_POINT ( 'NONE', #7572 ) ;
#7153 = CARTESIAN_POINT ( 'NONE',  ( 7.020400357098326438, 67.03996959729664695, 21.91068717264825239 ) ) ;
#7154 = CARTESIAN_POINT ( 'NONE',  ( 15.20622923973939677, 53.16901270175023342, 14.02455805003628520 ) ) ;
#7155 = DIRECTION ( 'NONE',  ( -1.000000000000000000, 0.000000000000000000, 0.000000000000000000 ) ) ;
#7156 = CARTESIAN_POINT ( 'NONE',  ( 53.00000000000000000, 51.46446609406726935, 3.535533905932731091 ) ) ;
#7157 = CARTESIAN_POINT ( 'NONE',  ( -78.00000000000001421, 54.99999999999998579, -8.485278002320759683 ) ) ;
#7158 = CARTESIAN_POINT ( 'NONE',  ( -75.21875000204839523, 36.74823131438024859, -18.25176868561973720 ) ) ;
#7159 = ORIENTED_EDGE ( 'NONE', *, *, #9027, .T. ) ;
#7160 = CARTESIAN_POINT ( 'NONE',  ( -78.00000000000001421, 42.27207793864211283, -12.72791868944003824 ) ) ;
#7161 = CARTESIAN_POINT ( 'NONE',  ( -75.03125000204839523, 36.74823131438024859, -18.25176868561973720 ) ) ;
#7162 = CARTESIAN_POINT ( 'NONE',  ( -78.00000000000001421, 67.72792206135787296, -4.242637315201482906 ) ) ;
#7163 = CARTESIAN_POINT ( 'NONE',  ( 0.000000000000000000, 0.000000000000000000, -2.617914285714285416 ) ) ;
#7164 = CARTESIAN_POINT ( 'NONE',  ( -0.4260572601936686854, 54.99150886132364491, -0.02483499414063310151 ) ) ;
#7165 =( NAMED_UNIT ( * ) SI_UNIT ( $, .STERADIAN. ) SOLID_ANGLE_UNIT ( ) );
#7166 = CARTESIAN_POINT ( 'NONE',  ( -74.99999999999997158, 35.03849855854433315, 15.32554794922328156 ) ) ;
#7167 = ORIENTED_EDGE ( 'NONE', *, *, #5230, .T. ) ;
#7168 = DIRECTION ( 'NONE',  ( 0.000000000000000000, 1.000000000000000000, 0.000000000000000000 ) ) ;
#7169 = AXIS2_PLACEMENT_3D ( 'NONE', #752, #10754, #3339 ) ;
#7170 = CARTESIAN_POINT ( 'NONE',  ( -67.17448730496187181, 36.66801277209461318, 10.55271442276269944 ) ) ;
#7171 = ORIENTED_EDGE ( 'NONE', *, *, #668, .T. ) ;
#7172 = CARTESIAN_POINT ( 'NONE',  ( -41.36397681821770078, 53.96873918909963663, -20.99311060721154121 ) ) ;
#7173 = CARTESIAN_POINT ( 'NONE',  ( -77.84375000204839523, 73.25176868561975141, -18.25176868561974430 ) ) ;
#7174 = EDGE_LOOP ( 'NONE', ( #10747, #8294, #7859, #11142 ) ) ;
#7175 = CARTESIAN_POINT ( 'NONE',  ( -74.56250000204839523, 80.81189881250001861, 10.69163855873948599 ) ) ;
#7176 = DIRECTION ( 'NONE',  ( -1.000000000000000000, -0.000000000000000000, -0.000000000000000000 ) ) ;
#7177 = PRESENTATION_STYLE_ASSIGNMENT (( #2271 ) ) ;
#7178 = ADVANCED_FACE ( 'NONE', ( #363 ), #7745, .F. ) ;
#7179 = ORIENTED_EDGE ( 'NONE', *, *, #11407, .F. ) ;
#7180 = DIRECTION ( 'NONE',  ( -1.000000000000000000, 0.000000000000000000, 0.000000000000000000 ) ) ;
#7181 = CARTESIAN_POINT ( 'NONE',  ( 25.37133272033247877, 59.99999999999997158, 0.3324664797073844102 ) ) ;
#7182 = CARTESIAN_POINT ( 'NONE',  ( 4.496465067834011009, 55.00390890337079242, 0.0002487324669923884337 ) ) ;
#7183 = ORIENTED_EDGE ( 'NONE', *, *, #9645, .T. ) ;
#7184 = CARTESIAN_POINT ( 'NONE',  ( 8.811013807768157236, 36.66975794146507184, 10.56480398736207960 ) ) ;
#7185 = CARTESIAN_POINT ( 'NONE',  ( -38.47762819156672265, 42.07891330237754346, -16.80402559754432801 ) ) ;
#7186 = DIRECTION ( 'NONE',  ( 0.000000000000000000, 0.000000000000000000, -1.000000000000000000 ) ) ;
#7187 = DIRECTION ( 'NONE',  ( -1.000000000000000000, 0.000000000000000000, 0.000000000000000000 ) ) ;
#7188 = DIRECTION ( 'NONE',  ( 0.000000000000000000, 0.000000000000000000, 1.000000000000000000 ) ) ;
#7189 = EDGE_LOOP ( 'NONE', ( #7238, #9695, #11164, #290 ) ) ;
#7190 = CARTESIAN_POINT ( 'NONE',  ( -76.53125000000004263, 79.99999999999990052, 10.35533905932733312 ) ) ;
#7191 = DIRECTION ( 'NONE',  ( 0.000000000000000000, 1.000000000000000000, 0.000000000000000000 ) ) ;
#7192 = FACE_BOUND ( 'NONE', #583, .T. ) ;
#7193 = EDGE_CURVE ( 'NONE', #1626, #9767, #1329, .T. ) ;
#7194 = AXIS2_PLACEMENT_3D ( 'NONE', #6585, #1292, #2976 ) ;
#7195 = ADVANCED_FACE ( 'NONE', ( #10308 ), #9597, .F. ) ;
#7196 = CARTESIAN_POINT ( 'NONE',  ( -53.73751484135783585, 71.24472392590685388, 13.33357819947211453 ) ) ;
#7197 = EDGE_CURVE ( 'NONE', #1659, #66, #3659, .T. ) ;
#7198 = EDGE_LOOP ( 'NONE', ( #4310, #6298 ) ) ;
#7199 = DIRECTION ( 'NONE',  ( -1.000000000000000000, -0.000000000000000000, -0.000000000000000000 ) ) ;
#7200 = DIRECTION ( 'NONE',  ( 0.000000000000000000, 0.000000000000000000, 1.000000000000000000 ) ) ;
#7201 = ORIENTED_EDGE ( 'NONE', *, *, #1731, .T. ) ;
#7202 = FACE_OUTER_BOUND ( 'NONE', #4646, .T. ) ;
#7203 = EDGE_CURVE ( 'NONE', #4769, #6710, #1206, .T. ) ;
#7204 = ADVANCED_FACE ( 'NONE', ( #8522 ), #10545, .F. ) ;
#7205 = DIRECTION ( 'NONE',  ( 0.000000000000000000, -0.000000000000000000, -1.000000000000000000 ) ) ;
#7206 = CARTESIAN_POINT ( 'NONE',  ( -76.81250000204838102, 29.18810118750000626, -10.69163855873949309 ) ) ;
#7207 = CARTESIAN_POINT ( 'NONE',  ( -78.96875000204839523, 73.25176868561975141, 18.25176868561974075 ) ) ;
#7208 = AXIS2_PLACEMENT_3D ( 'NONE', #2508, #8912, #5146 ) ;
#7209 = EDGE_LOOP ( 'NONE', ( #5197, #3698, #5538, #4336 ) ) ;
#7210 = EDGE_CURVE ( 'NONE', #518, #5239, #244, .T. ) ;
#7211 = CARTESIAN_POINT ( 'NONE',  ( 52.99999999999999289, 55.00000000000000000, 0.000000000000000000 ) ) ;
#7212 = ORIENTED_EDGE ( 'NONE', *, *, #4525, .T. ) ;
#7213 = CARTESIAN_POINT ( 'NONE',  ( 1.722085729088277395, 65.52543047797470877, 22.67635561717434811 ) ) ;
#7214 = CARTESIAN_POINT ( 'NONE',  ( 17.53948780091567983, 58.67519633682641000, 13.65775887405797029 ) ) ;
#7215 = CARTESIAN_POINT ( 'NONE',  ( -77.84375000204839523, 55.00000000000000000, -25.81189881249999729 ) ) ;
#7216 = DIRECTION ( 'NONE',  ( -1.000000000000000000, -0.000000000000000000, -0.000000000000000000 ) ) ;
#7217 = LINE ( 'NONE', #11684, #6675 ) ;
#7218 = CARTESIAN_POINT ( 'NONE',  ( -74.28125000204838102, 55.00000000000000000, 25.81189881249999729 ) ) ;
#7219 = EDGE_LOOP ( 'NONE', ( #4877, #9251 ) ) ;
#7220 = CIRCLE ( 'NONE', #2032, 1.500000000000001332 ) ;
#7221 = CYLINDRICAL_SURFACE ( 'NONE', #1441, 1.499999999999999556 ) ;
#7222 = CARTESIAN_POINT ( 'NONE',  ( -72.68750000204839523, 65.69163855873949842, 25.81189881250000440 ) ) ;
#7223 = CARTESIAN_POINT ( 'NONE',  ( -78.00000000000002842, 42.27207793864211283, 11.22792543327562775 ) ) ;
#7224 = LINE ( 'NONE', #3612, #5786 ) ;
#7225 = CARTESIAN_POINT ( 'NONE',  ( -41.95224010427075001, 55.00407356838249484, -0.007580890217307994366 ) ) ;
#7226 = CONTEXT_DEPENDENT_SHAPE_REPRESENTATION ( #8382, #11115 ) ;
#7227 = CARTESIAN_POINT ( 'NONE',  ( -15.35976620422333205, 71.92262103984167254, -14.06847932524695821 ) ) ;
#7228 = VECTOR ( 'NONE', #8578, 1000.000000000000000 ) ;
#7229 = ORIENTED_EDGE ( 'NONE', *, *, #4691, .F. ) ;
#7230 = CARTESIAN_POINT ( 'NONE',  ( -13.12643311661332746, 59.84143854988970190, 1.290711584744844043 ) ) ;
#7231 = AXIS2_PLACEMENT_3D ( 'NONE', #1102, #11338, #5614 ) ;
#7232 = CARTESIAN_POINT ( 'NONE',  ( -65.06671514604981610, 41.61929618219224380, 16.30332023460171698 ) ) ;
#7233 = VERTEX_POINT ( 'NONE', #305 ) ;
#7234 = CARTESIAN_POINT ( 'NONE',  ( -19.78535886778656661, 65.80747357543212672, 18.02991983063459003 ) ) ;
#7235 = CARTESIAN_POINT ( 'NONE',  ( -74.46875000204839523, 73.25176868561975141, 18.25176868561974075 ) ) ;
#7236 = AXIS2_PLACEMENT_3D ( 'NONE', #2375, #9510, #6050 ) ;
#7237 = PRESENTATION_LAYER_ASSIGNMENT (  '', '', ( #6669 ) ) ;
#7238 = ORIENTED_EDGE ( 'NONE', *, *, #5200, .T. ) ;
#7239 = CARTESIAN_POINT ( 'NONE',  ( -71.48947498017410851, 75.17259594761931396, 16.68383898576512081 ) ) ;
#7240 = CARTESIAN_POINT ( 'NONE',  ( -25.52231952398968673, 42.10919693116569817, 16.77412918608628090 ) ) ;
#7241 = ADVANCED_FACE ( 'NONE', ( #3537 ), #8820, .F. ) ;
#7242 = DIRECTION ( 'NONE',  ( 1.000000000000000000, 0.000000000000000000, 0.000000000000000000 ) ) ;
#7243 = CARTESIAN_POINT ( 'NONE',  ( 20.42601516676554851, 54.98551770566741936, -0.007780136594349751702 ) ) ;
#7244 = CIRCLE ( 'NONE', #2059, 1.500000000000001332 ) ;
#7245 = EDGE_LOOP ( 'NONE', ( #4636, #3818, #1094, #10976 ) ) ;
#7246 = CARTESIAN_POINT ( 'NONE',  ( -59.00490307935969270, 55.00061426705308065, 21.02882928537637497 ) ) ;
#7247 = CARTESIAN_POINT ( 'NONE',  ( -24.47759590008010377, 52.25445690686086664, 21.01882782503509262 ) ) ;
#7248 =( NAMED_UNIT ( * ) PLANE_ANGLE_UNIT ( ) SI_UNIT ( $, .RADIAN. ) );
#7249 = CARTESIAN_POINT ( 'NONE',  ( -78.00000000000002842, 42.27207793864211283, 5.742644059037075088 ) ) ;
#7250 = CYLINDRICAL_SURFACE ( 'NONE', #6518, 1.499999999999999556 ) ;
#7251 = ORIENTED_EDGE ( 'NONE', *, *, #8182, .F. ) ;
#7252 = CARTESIAN_POINT ( 'NONE',  ( -93.29762528721818171, 110.0087426977633669, -0.02929211074601270615 ) ) ;
#7253 = DIRECTION ( 'NONE',  ( 1.000000000000000000, 0.000000000000000000, -0.000000000000000000 ) ) ;
#7254 = CARTESIAN_POINT ( 'NONE',  ( -54.34438039152910704, 58.05280871788295372, 3.973341673354612524 ) ) ;
#7255 = VECTOR ( 'NONE', #822, 1000.000000000000000 ) ;
#7256 = ORIENTED_EDGE ( 'NONE', *, *, #2521, .T. ) ;
#7257 = CARTESIAN_POINT ( 'NONE',  ( -55.14769694417690715, 59.49448256121726786, 2.215039651009127031 ) ) ;
#7258 = ORIENTED_EDGE ( 'NONE', *, *, #9059, .T. ) ;
#7259 = CARTESIAN_POINT ( 'NONE',  ( 36.99999999999999289, 55.00000000000000000, -5.249999999999998224 ) ) ;
#7260 = DIRECTION ( 'NONE',  ( -1.000000000000000000, 0.000000000000000000, 0.000000000000000000 ) ) ;
#7261 = FACE_OUTER_BOUND ( 'NONE', #9892, .T. ) ;
#7262 = CARTESIAN_POINT ( 'NONE',  ( -75.03125000204838102, 55.00000000000000000, -25.81189881249999729 ) ) ;
#7263 = CARTESIAN_POINT ( 'NONE',  ( -78.31250000204838102, 29.18810118750000626, -10.69163855873949309 ) ) ;
#7264 = VERTEX_POINT ( 'NONE', #7151 ) ;
#7265 = CARTESIAN_POINT ( 'NONE',  ( -74.65625000204839523, 73.25176868561975141, -18.25176868561974430 ) ) ;
#7266 = ORIENTED_EDGE ( 'NONE', *, *, #9234, .T. ) ;
#7267 = CARTESIAN_POINT ( 'NONE',  ( 21.38655605994216558, 76.71840771742046172, 12.40410437900267127 ) ) ;
#7268 = CARTESIAN_POINT ( 'NONE',  ( -12.79377121657755190, 69.02455796469044458, 1.830988287285042926 ) ) ;
#7269 = ADVANCED_FACE ( 'NONE', ( #7864 ), #1676, .T. ) ;
#7270 = CARTESIAN_POINT ( 'NONE',  ( -76.90625000204839523, 36.74823131438026280, 18.25176868561974786 ) ) ;
#7271 = CARTESIAN_POINT ( 'NONE',  ( -78.00000000000001421, 67.72792206135787296, -12.72791868944004534 ) ) ;
#7272 = CARTESIAN_POINT ( 'NONE',  ( 6.123233995736766282E-16, -30.00000000000000000, 5.000000000000000000 ) ) ;
#7273 = AXIS2_PLACEMENT_3D ( 'NONE', #10047, #11843, #8386 ) ;
#7274 = AXIS2_PLACEMENT_3D ( 'NONE', #7791, #4191, #4813 ) ;
#7275 = ORIENTED_EDGE ( 'NONE', *, *, #2800, .T. ) ;
#7276 = CARTESIAN_POINT ( 'NONE',  ( -75.87500000409677625, 55.00000000000000000, -24.99999999999999645 ) ) ;
#7277 = CARTESIAN_POINT ( 'NONE',  ( -71.84375000204838102, 55.00000000000000000, -25.81189881249999729 ) ) ;
#7278 = EDGE_CURVE ( 'NONE', #5122, #8651, #11677, .T. ) ;
#7279 = DIRECTION ( 'NONE',  ( -1.000000000000000000, -0.000000000000000000, -0.000000000000000000 ) ) ;
#7280 = CARTESIAN_POINT ( 'NONE',  ( -63.42686368473390957, 54.98038842139913385, 0.01519274601354845579 ) ) ;
#7281 = CONTEXT_DEPENDENT_SHAPE_REPRESENTATION ( #4326, #2906 ) ;
#7282 = VECTOR ( 'NONE', #10595, 1000.000000000000000 ) ;
#7283 = CARTESIAN_POINT ( 'NONE',  ( -21.12429042622422060, 76.50559246739102548, 4.651484971764126009 ) ) ;
#7284 = CARTESIAN_POINT ( 'NONE',  ( -14.68353320191416067, 59.33897812137291794, 2.505989342657766628 ) ) ;
#7285 = EDGE_LOOP ( 'NONE', ( #1162, #9316, #7615, #3091 ) ) ;
#7286 = CARTESIAN_POINT ( 'NONE',  ( -78.00000000000000000, 55.00000000000000000, 21.50000000000000000 ) ) ;
#7287 = ORIENTED_EDGE ( 'NONE', *, *, #10188, .F. ) ;
#7288 = CARTESIAN_POINT ( 'NONE',  ( 12.85570563148687739, 52.25434904275299175, 21.01882863504484789 ) ) ;
#7289 = AXIS2_PLACEMENT_3D ( 'NONE', #2296, #2409, #8768 ) ;
#7290 = CARTESIAN_POINT ( 'NONE',  ( -76.15625000204839523, 73.25176868561975141, -18.25176868561974430 ) ) ;
#7291 = EDGE_LOOP ( 'NONE', ( #3558, #8379 ) ) ;
#7292 = CARTESIAN_POINT ( 'NONE',  ( -72.78125000204838102, 55.00000000000000000, 25.81189881249999729 ) ) ;
#7293 = CARTESIAN_POINT ( 'NONE',  ( 0.1442708919848544047, 44.43605983923426805, -18.32883121229183487 ) ) ;
#7294 = AXIS2_PLACEMENT_3D ( 'NONE', #7104, #1516, #6144 ) ;
#7295 = ADVANCED_FACE ( 'NONE', ( #11737 ), #3486, .T. ) ;
#7296 = ORIENTED_EDGE ( 'NONE', *, *, #11176, .T. ) ;
#7297 = VECTOR ( 'NONE', #10351, 1000.000000000000000 ) ;
#7298 = DIRECTION ( 'NONE',  ( -1.000000000000000000, 0.000000000000000000, 0.000000000000000000 ) ) ;
#7299 = CARTESIAN_POINT ( 'NONE',  ( -10.09032851302145950, 54.99509807286066376, 0.004314335854857118992 ) ) ;
#7300 = EDGE_LOOP ( 'NONE', ( #11002, #7505, #1128, #10376 ) ) ;
#7301 = CARTESIAN_POINT ( 'NONE',  ( -59.36500404872999326, 56.03206174438126652, 20.99316529255160191 ) ) ;
#7302 = AXIS2_PLACEMENT_3D ( 'NONE', #4865, #3902, #1254 ) ;
#7303 = CARTESIAN_POINT ( 'NONE',  ( 3.451907635234679361, 34.19915017745972108, -3.085386652995293133 ) ) ;
#7304 = DIRECTION ( 'NONE',  ( 0.000000000000000000, 0.000000000000000000, 1.000000000000000000 ) ) ;
#7305 = CARTESIAN_POINT ( 'NONE',  ( 0.000000000000000000, 0.000000000000000000, -6.074599999999999334 ) ) ;
#7306 = CARTESIAN_POINT ( 'NONE',  ( 3.000000000000000888, 3.673940397442060854E-16, -6.074599999999999334 ) ) ;
#7307 = DIRECTION ( 'NONE',  ( -1.000000000000000000, 0.000000000000000000, 0.000000000000000000 ) ) ;
#7308 = ORIENTED_EDGE ( 'NONE', *, *, #8281, .F. ) ;
#7309 = DIRECTION ( 'NONE',  ( -0.000000000000000000, -0.000000000000000000, -1.000000000000000000 ) ) ;
#7310 = CARTESIAN_POINT ( 'NONE',  ( -51.90718173048562534, 54.98364889560268409, -0.001639402367017143113 ) ) ;
#7311 = CARTESIAN_POINT ( 'NONE',  ( -38.01415270387070677, 53.70170271778372495, -4.839460789004083274 ) ) ;
#7312 = CONICAL_SURFACE ( 'NONE', #222, 5.000000000000000888, 1.047197551196596299 ) ;
#7313 = CARTESIAN_POINT ( 'NONE',  ( -80.00000000000000000, 55.00000000000000000, 25.00000000000000355 ) ) ;
#7314 = ADVANCED_FACE ( 'NONE', ( #771 ), #7032, .F. ) ;
#7315 = CARTESIAN_POINT ( 'NONE',  ( -74.46875000409679046, 44.64466094067277879, -25.00000000000015987 ) ) ;
#7316 = ORIENTED_EDGE ( 'NONE', *, *, #1692, .T. ) ;
#7317 = CARTESIAN_POINT ( 'NONE',  ( -2.500000000000000000, 3.061616997868383141E-16, -5.560532340533429263 ) ) ;
#7318 = FACE_OUTER_BOUND ( 'NONE', #7368, .T. ) ;
#7319 = CARTESIAN_POINT ( 'NONE',  ( 21.84682584988675202, 59.99999999999999289, 0.3320659484734538869 ) ) ;
#7320 = CARTESIAN_POINT ( 'NONE',  ( -73.53125000204838102, 55.00000000000000000, -25.81189881249999729 ) ) ;
#7321 = AXIS2_PLACEMENT_3D ( 'NONE', #2772, #5529, #4683 ) ;
#7322 = DIRECTION ( 'NONE',  ( -1.000000000000000000, -0.000000000000000000, -0.000000000000000000 ) ) ;
#7323 = ORIENTED_EDGE ( 'NONE', *, *, #6453, .T. ) ;
#7324 = FACE_BOUND ( 'NONE', #3196, .T. ) ;
#7325 = VERTEX_POINT ( 'NONE', #5344 ) ;
#7326 = LINE ( 'NONE', #10053, #10275 ) ;
#7327 = CARTESIAN_POINT ( 'NONE',  ( 22.20627439270837655, 67.25635803115373790, 7.058475852763654856 ) ) ;
#7328 = EDGE_CURVE ( 'NONE', #9312, #7933, #6252, .T. ) ;
#7329 = CARTESIAN_POINT ( 'NONE',  ( -78.59375000204839523, 55.00000000000000000, 25.81189881249999729 ) ) ;
#7330 = CARTESIAN_POINT ( 'NONE',  ( -78.96875000000001421, 30.00000000000003908, 10.35533905932737753 ) ) ;
#7331 = LINE ( 'NONE', #6428, #1289 ) ;
#7332 = VERTEX_POINT ( 'NONE', #9651 ) ;
#7333 = CARTESIAN_POINT ( 'NONE',  ( -78.00000000000002842, 50.75735931288069480, 4.242644059037076865 ) ) ;
#7334 = CARTESIAN_POINT ( 'NONE',  ( -75.03125000409677625, 44.64466094067262958, 25.00000000000001066 ) ) ;
#7335 = LINE ( 'NONE', #10008, #4604 ) ;
#7336 = CARTESIAN_POINT ( 'NONE',  ( -57.71391471235212123, 54.99984036959516942, -0.007998007078910979867 ) ) ;
#7337 = ITEM_DEFINED_TRANSFORMATION ( 'NONE', 'NONE', #6807,  #4738 ) ;
#7338 = EDGE_CURVE ( 'NONE', #2315, #818, #5283, .T. ) ;
#7339 = PLANE ( 'NONE',  #7120 ) ;
#7340 = EDGE_CURVE ( 'NONE', #1874, #8687, #4448, .T. ) ;
#7341 = CARTESIAN_POINT ( 'NONE',  ( -24.79786866689667946, 51.95154789264624640, 3.976631450565629500 ) ) ;
#7342 = ORIENTED_EDGE ( 'NONE', *, *, #542, .T. ) ;
#7343 = CARTESIAN_POINT ( 'NONE',  ( -78.00000000000002842, 54.99999999999998579, 18.47056612039490986 ) ) ;
#7344 = VERTEX_POINT ( 'NONE', #9709 ) ;
#7345 = CARTESIAN_POINT ( 'NONE',  ( 2.595920079249742329, 34.88763922991881827, -6.102757042485290384 ) ) ;
#7346 = CARTESIAN_POINT ( 'NONE',  ( -78.50000000204840944, 44.30836144126053000, 25.81189881250000795 ) ) ;
#7347 = ADVANCED_FACE ( 'NONE', ( #9880 ), #6923, .F. ) ;
#7348 = ORIENTED_EDGE ( 'NONE', *, *, #931, .F. ) ;
#7349 = EDGE_CURVE ( 'NONE', #4551, #1195, #10345, .T. ) ;
#7350 = CARTESIAN_POINT ( 'NONE',  ( -73.43750000204839523, 65.69163855873948421, -25.81189881250000440 ) ) ;
#7351 = CARTESIAN_POINT ( 'NONE',  ( -38.60828084422895046, 48.85949782923615459, -20.20603288453101243 ) ) ;
#7352 = EDGE_LOOP ( 'NONE', ( #2267, #4321, #5232, #10966 ) ) ;
#7353 = DIRECTION ( 'NONE',  ( -0.000000000000000000, -0.000000000000000000, 1.000000000000000000 ) ) ;
#7354 = CARTESIAN_POINT ( 'NONE',  ( 13.42607030714540706, 55.00164660868858135, -0.01635937553770835245 ) ) ;
#7355 = VERTEX_POINT ( 'NONE', #11617 ) ;
#7356 = CARTESIAN_POINT ( 'NONE',  ( -25.47762819357030395, 44.41853719948864665, 18.37117470573356925 ) ) ;
#7357 = CARTESIAN_POINT ( 'NONE',  ( -32.11869219899978845, 34.20636958863568822, 3.085052597841025701 ) ) ;
#7358 = CARTESIAN_POINT ( 'NONE',  ( -5.000000000000000000, 2.886751345948134428, -5.653418012614792154 ) ) ;
#7359 = FACE_OUTER_BOUND ( 'NONE', #1470, .T. ) ;
#7360 = DIRECTION ( 'NONE',  ( -1.000000000000000000, 0.000000000000000000, 0.000000000000000000 ) ) ;
#7361 = CARTESIAN_POINT ( 'NONE',  ( 0.000000000000000000, 0.000000000000000000, 0.000000000000000000 ) ) ;
#7362 = ORIENTED_EDGE ( 'NONE', *, *, #8927, .F. ) ;
#7363 = DIRECTION ( 'NONE',  ( -1.000000000000000000, -0.000000000000000000, -0.000000000000000000 ) ) ;
#7364 = CARTESIAN_POINT ( 'NONE',  ( -56.46182468818901157, 54.99756168373090048, -0.002722472456010964752 ) ) ;
#7365 = CARTESIAN_POINT ( 'NONE',  ( -60.76133702166824690, 52.93822791804927164, 4.558078328184683947 ) ) ;
#7366 = CYLINDRICAL_SURFACE ( 'NONE', #3856, 4.999999999999984013 ) ;
#7367 = DIRECTION ( 'NONE',  ( -1.000000000000000000, -0.000000000000000000, -0.000000000000000000 ) ) ;
#7368 = EDGE_LOOP ( 'NONE', ( #7733, #4449, #9724, #3055 ) ) ;
#7369 = CARTESIAN_POINT ( 'NONE',  ( 21.14436220910852882, 71.77416011014268804, 12.89076390558360075 ) ) ;
#7370 = CARTESIAN_POINT ( 'NONE',  ( -80.00000000000002842, 42.27207793864211283, 11.22792543327562775 ) ) ;
#7371 = DIRECTION ( 'NONE',  ( -1.000000000000000000, 0.000000000000000000, 0.000000000000000000 ) ) ;
#7372 = CARTESIAN_POINT ( 'NONE',  ( -73.25000000204838102, 80.81189881250001861, -10.69163855873949132 ) ) ;
#7373 = CARTESIAN_POINT ( 'NONE',  ( -78.59375000204839523, 36.74823131438026280, 18.25176868561974786 ) ) ;
#7374 = PRESENTATION_LAYER_ASSIGNMENT (  '', '', ( #1440 ) ) ;
#7375 = ORIENTED_EDGE ( 'NONE', *, *, #9946, .F. ) ;
#7376 = CARTESIAN_POINT ( 'NONE',  ( -75.59375000204839523, 55.00000000000000000, 25.81189881249999729 ) ) ;
#7377 = ORIENTED_EDGE ( 'NONE', *, *, #10786, .T. ) ;
#7378 = CARTESIAN_POINT ( 'NONE',  ( 5.849089671321329398, 66.56396111897267076, 22.16541920639843255 ) ) ;
#7379 = CARTESIAN_POINT ( 'NONE',  ( 3.163514083425913892, 43.29694055639052408, -7.813017536009592590 ) ) ;
#7380 = B_SPLINE_CURVE_WITH_KNOTS ( 'NONE', 3,
 ( #11534, #521, #1598, #3284, #695, #6954, #3467, #1543 ),
 .UNSPECIFIED., .F., .F.,
 ( 4, 2, 2, 4 ),
 ( 0.002921158011986708155, 0.003648658599403066180, 0.004376159186819424639, 0.005831160361652140689 ),
 .UNSPECIFIED. ) ;
#7381 = CARTESIAN_POINT ( 'NONE',  ( 39.99999999999999289, 55.00000000000000000, 0.000000000000000000 ) ) ;
#7382 = ADVANCED_FACE ( 'NONE', ( #1505 ), #9775, .F. ) ;
#7383 = CARTESIAN_POINT ( 'NONE',  ( -75.00000000000000000, 69.43970489681053948, -21.16564186330591468 ) ) ;
#7384 = FACE_OUTER_BOUND ( 'NONE', #4211, .T. ) ;
#7385 = EDGE_LOOP ( 'NONE', ( #1203, #7599, #1448, #7582 ) ) ;
#7386 = CARTESIAN_POINT ( 'NONE',  ( -74.09375000000007105, 44.64466094067265800, -24.99999999999985434 ) ) ;
#7387 = CARTESIAN_POINT ( 'NONE',  ( -71.40810441781462714, 80.81189881250000440, 6.916273779317701376 ) ) ;
#7388 = FACE_OUTER_BOUND ( 'NONE', #7385, .T. ) ;
#7389 = CARTESIAN_POINT ( 'NONE',  ( -53.61888101636234438, 55.00545574595133047, 0.006701513939034802261 ) ) ;
#7390 = APPLICATION_PROTOCOL_DEFINITION ( 'draft international standard', 'automotive_design', 1998, #10888 ) ;
#7391 = CARTESIAN_POINT ( 'NONE',  ( -18.38663302488769347, 74.26727426732456649, 10.62400905199263690 ) ) ;
#7392 = CIRCLE ( 'NONE', #2222, 1.500000000000001332 ) ;
#7393 = CARTESIAN_POINT ( 'NONE',  ( 47.00000000000000000, 55.00000000000000000, 0.000000000000000000 ) ) ;
#7394 =( BOUNDED_CURVE ( )  B_SPLINE_CURVE ( 2, ( #689, #8013, #11651, #8343, #1932, #1991, #10377, #129, #3793 ),
 .UNSPECIFIED., .F., .T. ) 
 B_SPLINE_CURVE_WITH_KNOTS ( ( 3, 2, 2, 2, 3 ),
 ( 0.000000000000000000, 0.01979916996583446290, 0.03959833993166892580, 0.05939750989750339216, 0.07919667986333785159 ),
 .UNSPECIFIED. ) 
 CURVE ( )  GEOMETRIC_REPRESENTATION_ITEM ( )  RATIONAL_B_SPLINE_CURVE ( ( 1.000000000000000000, 0.9238795325112868495, 1.000000000000000000, 0.9238795325112868495, 1.000000000000000000, 0.9238795325112868495, 1.000000000000000000, 0.9238795325112868495, 1.000000000000000000 ) ) 
 REPRESENTATION_ITEM ( '' )  );
#7395 = VERTEX_POINT ( 'NONE', #3419 ) ;
#7396 = DIRECTION ( 'NONE',  ( -0.000000000000000000, -1.000000000000000000, -0.000000000000000000 ) ) ;
#7397=STYLED_ITEM('',(#11902),#8587);
#7398 = CARTESIAN_POINT ( 'NONE',  ( -74.00000000409677625, 80.00000000000000000, -1.530808498934191324E-15 ) ) ;
#7399 = ORIENTED_EDGE ( 'NONE', *, *, #1321, .F. ) ;
#7400 = CARTESIAN_POINT ( 'NONE',  ( -69.67438043473205767, 33.99524309754638551, 0.006656162479001280670 ) ) ;
#7401 = CARTESIAN_POINT ( 'NONE',  ( -72.31250000204839523, 29.18810118750000626, -10.69163855873949309 ) ) ;
#7402 = VERTEX_POINT ( 'NONE', #8936 ) ;
#7403 = PRODUCT ( 'Crank Handle', 'Crank Handle', '', ( #4574 ) ) ;
#7404 = CARTESIAN_POINT ( 'NONE',  ( -71.53052369147286527, 77.35376373433385311, 12.90594309674112949 ) ) ;
#7405 = CARTESIAN_POINT ( 'NONE',  ( -40.03064391692543467, 53.96877717286832876, -20.99202776130344361 ) ) ;
#7406 = VECTOR ( 'NONE', #9713, 1000.000000000000114 ) ;
#7407 = SURFACE_STYLE_FILL_AREA ( #2674 ) ;
#7408 = CARTESIAN_POINT ( 'NONE',  ( 47.00000000000000000, 105.0000000000000142, 6.000000000000000000 ) ) ;
#7409 = ORIENTED_EDGE ( 'NONE', *, *, #9746, .F. ) ;
#7410 = EDGE_CURVE ( 'NONE', #4040, #5487, #11685, .T. ) ;
#7411 = CARTESIAN_POINT ( 'NONE',  ( -72.50000000409677625, 80.00000000000000000, -1.530808498934191324E-15 ) ) ;
#7412 = CARTESIAN_POINT ( 'NONE',  ( -77.84374999999997158, 65.35533905932209109, 25.00000000000518341 ) ) ;
#7413 = ORIENTED_EDGE ( 'NONE', *, *, #11763, .F. ) ;
#7414 = CARTESIAN_POINT ( 'NONE',  ( -19.40408043161419371, 64.90577468530469218, 18.53575269199317788 ) ) ;
#7415 = VECTOR ( 'NONE', #2558, 1000.000000000000114 ) ;
#7416 = CARTESIAN_POINT ( 'NONE',  ( -52.27495405780593529, 76.01412898031726684, 2.059423305703688811 ) ) ;
#7417 = CARTESIAN_POINT ( 'NONE',  ( -73.15625000409679046, 30.00000000000000355, -10.35533905932738108 ) ) ;
#7418 = CARTESIAN_POINT ( 'NONE',  ( 0.000000000000000000, 0.000000000000000000, -4.346257142857142597 ) ) ;
#7419 = CIRCLE ( 'NONE', #11797, 1.500000000000001332 ) ;
#7420 = FACE_OUTER_BOUND ( 'NONE', #11284, .T. ) ;
#7421 = ADVANCED_FACE ( 'NONE', ( #2348 ), #540, .F. ) ;
#7422 = CARTESIAN_POINT ( 'NONE',  ( 36.99999999999999289, 55.00000000000000000, 0.000000000000000000 ) ) ;
#7423 = EDGE_CURVE ( 'NONE', #322, #7683, #2120, .T. ) ;
#7424 = ORIENTED_EDGE ( 'NONE', *, *, #4555, .F. ) ;
#7425 = CARTESIAN_POINT ( 'NONE',  ( -71.18750000409677625, 72.67766952966368876, -17.67766952966368876 ) ) ;
#7426 = CARTESIAN_POINT ( 'NONE',  ( -34.00213111530580079, 55.00182194974264860, 0.0002174257210376325542 ) ) ;
#7427 = CARTESIAN_POINT ( 'NONE',  ( -34.51742062993405824, 51.23169754889989491, -3.302621543381780711 ) ) ;
#7428 = LINE ( 'NONE', #2863, #11258 ) ;
#7429 = CIRCLE ( 'NONE', #10471, 1.500000000000001332 ) ;
#7430 = CARTESIAN_POINT ( 'NONE',  ( -78.00000000000001421, 42.27207793864211283, -14.22791868944003646 ) ) ;
#7431 = CARTESIAN_POINT ( 'NONE',  ( -9.458587434131468186, 59.17210302956776502, -5.626626392890127448 ) ) ;
#7432 = ORIENTED_EDGE ( 'NONE', *, *, #7701, .T. ) ;
#7433 = DIRECTION ( 'NONE',  ( 0.000000000000000000, 1.000000000000000000, 0.000000000000000000 ) ) ;
#7434 = DIRECTION ( 'NONE',  ( -0.000000000000000000, -0.000000000000000000, 1.000000000000000000 ) ) ;
#7435 = PLANE ( 'NONE',  #5963 ) ;
#7436 = DIRECTION ( 'NONE',  ( 0.8191520442889974607, 1.003171929053531649E-16, -0.5735764363510379438 ) ) ;
#7437 = CARTESIAN_POINT ( 'NONE',  ( -0.4307873465902548049, 65.42943686846950868, -22.72062601704910989 ) ) ;
#7438 = DIRECTION ( 'NONE',  ( -1.000000000000000000, -0.000000000000000000, -0.000000000000000000 ) ) ;
#7439 = AXIS2_PLACEMENT_3D ( 'NONE', #5351, #9003, #3546 ) ;
#7440 = ORIENTED_EDGE ( 'NONE', *, *, #10300, .F. ) ;
#7441 = CARTESIAN_POINT ( 'NONE',  ( -79.06250000204840944, 80.81189881250001861, -10.69163855873949132 ) ) ;
#7442 = ORIENTED_EDGE ( 'NONE', *, *, #11853, .F. ) ;
#7443 = CARTESIAN_POINT ( 'NONE',  ( 8.136848973421107800, 67.55742525566687107, -21.61847732402205580 ) ) ;
#7444 = DIRECTION ( 'NONE',  ( 1.000000000000000000, 6.033820786006286457E-17, 0.000000000000000000 ) ) ;
#7445 = CARTESIAN_POINT ( 'NONE',  ( -43.50315269332450185, 62.81301754493210154, -11.70305962917251819 ) ) ;
#7446 = CARTESIAN_POINT ( 'NONE',  ( -77.65625000204839523, 73.25176868561975141, -18.25176868561974430 ) ) ;
#7447 = EDGE_CURVE ( 'NONE', #10129, #11498, #1552, .T. ) ;
#7448 = CARTESIAN_POINT ( 'NONE',  ( -74.99999999999997158, 79.03756697387808572, 7.232545519770552822 ) ) ;
#7449 = LINE ( 'NONE', #2036, #1496 ) ;
#7450 = ORIENTED_EDGE ( 'NONE', *, *, #8952, .T. ) ;
#7451 = CARTESIAN_POINT ( 'NONE',  ( -79.81250000000001421, 72.67766952966368876, -17.67766952966368876 ) ) ;
#7452 = CARTESIAN_POINT ( 'NONE',  ( -72.21875000204838102, 29.18810118750000271, 4.741568889096522788E-15 ) ) ;
#7453 = AXIS2_PLACEMENT_3D ( 'NONE', #6048, #2502, #2319 ) ;
#7454 = CARTESIAN_POINT ( 'NONE',  ( -78.00000000000002842, 42.27207793864211283, 4.242644059037075976 ) ) ;
#7455 = FACE_BOUND ( 'NONE', #7697, .T. ) ;
#7456 = CARTESIAN_POINT ( 'NONE',  ( -60.61922519846778101, 54.99654146924289222, 0.007592002550234120892 ) ) ;
#7457 = PRODUCT_CONTEXT ( 'NONE', #4944, 'mechanical' ) ;
#7458 = CARTESIAN_POINT ( 'NONE',  ( -20.36561017906013404, 75.87354305742351812, -7.076759675131881977 ) ) ;
#7459 = AXIS2_PLACEMENT_3D ( 'NONE', #6403, #10872, #4540 ) ;
#7460 = CARTESIAN_POINT ( 'NONE',  ( -5.000000000000000888, 0.9828435001097621804, -6.056909652965543067 ) ) ;
#7461 = VECTOR ( 'NONE', #2336, 1000.000000000000000 ) ;
#7462 = ORIENTED_EDGE ( 'NONE', *, *, #733, .T. ) ;
#7463 = ADVANCED_FACE ( 'NONE', ( #7324, #5580 ), #9223, .T. ) ;
#7464 = CARTESIAN_POINT ( 'NONE',  ( -5.000000000000000000, -0.9724665692850886778, -6.058069561147902959 ) ) ;
#7465 = LINE ( 'NONE', #4638, #386 ) ;
#7466 = ORIENTED_EDGE ( 'NONE', *, *, #9828, .T. ) ;
#7467 = CARTESIAN_POINT ( 'NONE',  ( -63.84363901113670892, 43.28205526181564267, 17.55452879243513920 ) ) ;
#7468 = CARTESIAN_POINT ( 'NONE',  ( -76.81250000204839523, 29.18810118750000981, 10.69163855873950020 ) ) ;
#7469 = ADVANCED_FACE ( 'NONE', ( #1971 ), #10803, .F. ) ;
#7470 = VECTOR ( 'NONE', #7598, 1000.000000000000000 ) ;
#7471 = CIRCLE ( 'NONE', #2494, 1.500000000000001332 ) ;
#7472 = FACE_OUTER_BOUND ( 'NONE', #79, .T. ) ;
#7473 = CARTESIAN_POINT ( 'NONE',  ( -4.160267277967630406, 59.12176995062825569, -20.68921489609442332 ) ) ;
#7474 =( LENGTH_UNIT ( ) NAMED_UNIT ( * ) SI_UNIT ( .MILLI., .METRE. ) );
#7475 = CARTESIAN_POINT ( 'NONE',  ( -32.72515708217407138, 34.82695427582095959, -6.127117481167428714 ) ) ;
#7476 = ORIENTED_EDGE ( 'NONE', *, *, #7559, .T. ) ;
#7477 = CARTESIAN_POINT ( 'NONE',  ( 36.99999999999999289, 64.99999999999998579, 0.000000000000000000 ) ) ;
#7478 = DIRECTION ( 'NONE',  ( 1.000000000000000000, 0.000000000000000000, 0.000000000000000000 ) ) ;
#7479 = CARTESIAN_POINT ( 'NONE',  ( 7.477680471578420196, 36.66673471410030061, 10.56605622896702990 ) ) ;
#7480 = ORIENTED_EDGE ( 'NONE', *, *, #1294, .F. ) ;
#7481 = CARTESIAN_POINT ( 'NONE',  ( -39.27494750982320681, 48.85996770079779594, -20.20489819083377014 ) ) ;
#7482 = CARTESIAN_POINT ( 'NONE',  ( -47.81092963715463640, 71.80394787507084686, -12.92116392654651058 ) ) ;
#7483 = DIRECTION ( 'NONE',  ( 0.000000000000000000, 0.000000000000000000, 1.000000000000000000 ) ) ;
#7484 = DIRECTION ( 'NONE',  ( 0.000000000000000000, 1.000000000000000000, 0.000000000000000000 ) ) ;
#7485 = CARTESIAN_POINT ( 'NONE',  ( 0.000000000000000000, 0.000000000000000000, -4.860324802323723326 ) ) ;
#7486 = EDGE_CURVE ( 'NONE', #4282, #9278, #7014, .T. ) ;
#7487 = ORIENTED_EDGE ( 'NONE', *, *, #9461, .T. ) ;
#7488 = CARTESIAN_POINT ( 'NONE',  ( -78.78125000000001421, 30.00000000000000355, -10.35533905932738108 ) ) ;
#7489 = CARTESIAN_POINT ( 'NONE',  ( -42.17020159496552623, 54.99975127115207840, 0.003908898248491586742 ) ) ;
#7490 = CARTESIAN_POINT ( 'NONE',  ( -47.34878363292850878, 59.83931338121328025, -1.298758957765639321 ) ) ;
#7491 = CARTESIAN_POINT ( 'NONE',  ( -77.37500000000005684, 30.00000000000009592, 4.592425496802557801E-15 ) ) ;
#7492 = AXIS2_PLACEMENT_3D ( 'NONE', #9445, #7544, #153 ) ;
#7493 = CARTESIAN_POINT ( 'NONE',  ( -80.00000000000002842, 59.24264068711927678, 12.72792543327563131 ) ) ;
#7494 = CARTESIAN_POINT ( 'NONE',  ( 9.890116692599228543, 51.46809947807167873, 6.132390081685909600 ) ) ;
#7495 = VERTEX_POINT ( 'NONE', #1660 ) ;
#7496 = CARTESIAN_POINT ( 'NONE',  ( 5.451907626115248817, 34.19820075889870026, -3.085388827037094828 ) ) ;
#7497 = CARTESIAN_POINT ( 'NONE',  ( 2.500000000000000000, 0.000000000000000000, -6.099999999999999645 ) ) ;
#7498 = CARTESIAN_POINT ( 'NONE',  ( -5.000000000000000000, 0.000000000000000000, -6.099999999999999645 ) ) ;
#7499 = DIRECTION ( 'NONE',  ( 0.000000000000000000, 0.000000000000000000, -1.000000000000000000 ) ) ;
#7500 = CARTESIAN_POINT ( 'NONE',  ( -14.95549379722967487, 71.72953881524270514, -18.61174932058436582 ) ) ;
#7501 = CARTESIAN_POINT ( 'NONE',  ( -78.59375000204839523, 55.00000000000000000, 25.81189881249999729 ) ) ;
#7502 = VERTEX_POINT ( 'NONE', #7077 ) ;
#7503 = CARTESIAN_POINT ( 'NONE',  ( -76.15625000409677625, 30.00000000000000355, -10.35533905932738108 ) ) ;
#7504 = VECTOR ( 'NONE', #2841, 1000.000000000000000 ) ;
#7505 = ORIENTED_EDGE ( 'NONE', *, *, #72, .T. ) ;
#7506 = CARTESIAN_POINT ( 'NONE',  ( 25.02328063624275600, 79.77146175834676001, 3.399146611245127847 ) ) ;
#7507 = ADVANCED_FACE ( 'NONE', ( #9808 ), #5328, .F. ) ;
#7508 = CARTESIAN_POINT ( 'NONE',  ( -48.53950828781236737, 68.97547034813443645, -1.831174528873022345 ) ) ;
#7509 = LINE ( 'NONE', #10238, #780 ) ;
#7510 = DIRECTION ( 'NONE',  ( 0.000000000000000000, 0.000000000000000000, 1.000000000000000000 ) ) ;
#7511 = LINE ( 'NONE', #6734, #5331 ) ;
#7512 = VECTOR ( 'NONE', #4537, 1000.000000000000000 ) ;
#7513 = ORIENTED_EDGE ( 'NONE', *, *, #4979, .F. ) ;
#7514 = CARTESIAN_POINT ( 'NONE',  ( -78.78125000000001421, 30.00000000000000355, -10.35533905932738108 ) ) ;
#7515 = CARTESIAN_POINT ( 'NONE',  ( -71.93750000409677625, 37.32233047033631124, 17.67766952966369232 ) ) ;
#7516 = CARTESIAN_POINT ( 'NONE',  ( -35.70892724115440586, 50.25524874376613838, -1.610804148112624290 ) ) ;
#7517 = FACE_BOUND ( 'NONE', #2193, .T. ) ;
#7518 = CARTESIAN_POINT ( 'NONE',  ( -15.16689040116921916, 60.84304562314972742, 3.905604940474681985 ) ) ;
#7519 = CARTESIAN_POINT ( 'NONE',  ( 47.00000000000000000, 55.00000000000000000, -6.000000000000000000 ) ) ;
#7520 = CYLINDRICAL_SURFACE ( 'NONE', #8924, 4.999999999999997335 ) ;
#7521 = VERTEX_POINT ( 'NONE', #1777 ) ;
#7522 = CARTESIAN_POINT ( 'NONE',  ( -5.000000000000000000, 0.000000000000000000, -6.099999999999999645 ) ) ;
#7523 = CARTESIAN_POINT ( 'NONE',  ( 52.99999999999999289, 58.53553390593273065, 3.535533905932731091 ) ) ;
#7524 = ORIENTED_EDGE ( 'NONE', *, *, #5297, .F. ) ;
#7525 = CARTESIAN_POINT ( 'NONE',  ( -3.477628190354089099, 49.49309465598528845, -20.46958112014059950 ) ) ;
#7526 = CARTESIAN_POINT ( 'NONE',  ( -78.96875000204839523, 80.81189881250000440, -1.580522963032174394E-15 ) ) ;
#7527 = DIRECTION ( 'NONE',  ( 0.000000000000000000, 0.000000000000000000, 1.000000000000000000 ) ) ;
#7528 = CARTESIAN_POINT ( 'NONE',  ( -57.27472358375123207, 61.14040963541170015, 20.20590277145669234 ) ) ;
#7529 = CARTESIAN_POINT ( 'NONE',  ( -57.27472358375123207, 61.14040963541170015, 20.20590277145669234 ) ) ;
#7530 = ORIENTED_EDGE ( 'NONE', *, *, #6789, .F. ) ;
#7531 = CARTESIAN_POINT ( 'NONE',  ( -74.09375000204839523, 55.00000000000000000, 25.81189881249999729 ) ) ;
#7532 = FACE_OUTER_BOUND ( 'NONE', #2737, .T. ) ;
#7533 = ADVANCED_FACE ( 'NONE', ( #10876 ), #10038, .T. ) ;
#7534 = DIRECTION ( 'NONE',  ( 0.000000000000000000, 1.000000000000000000, 0.000000000000000000 ) ) ;
#7535 = ORIENTED_EDGE ( 'NONE', *, *, #7203, .T. ) ;
#7536 = CARTESIAN_POINT ( 'NONE',  ( -57.94139028520521606, 61.13994508777751236, 20.20477452650387207 ) ) ;
#7537 = CARTESIAN_POINT ( 'NONE',  ( -69.52691976458234535, 34.01892180236649921, 2.749684864678113794 ) ) ;
#7538 = DIRECTION ( 'NONE',  ( -1.000000000000000000, -0.000000000000000000, -0.000000000000000000 ) ) ;
#7539 = CARTESIAN_POINT ( 'NONE',  ( -77.84375000409677625, 30.00000000000001421, 10.35533905932739174 ) ) ;
#7540 = FACE_OUTER_BOUND ( 'NONE', #2899, .T. ) ;
#7541 = CARTESIAN_POINT ( 'NONE',  ( 73.00000000000000000, 102.0481555856608225, -9.797174393178809880E-16 ) ) ;
#7542 = EDGE_CURVE ( 'NONE', #8959, #11839, #6527, .T. ) ;
#7543 = ORIENTED_EDGE ( 'NONE', *, *, #6690, .T. ) ;
#7544 = DIRECTION ( 'NONE',  ( 0.000000000000000000, 1.000000000000000000, 0.000000000000000000 ) ) ;
#7545 = DIRECTION ( 'NONE',  ( 0.000000000000000000, 0.000000000000000000, 1.000000000000000000 ) ) ;
#7546 = CARTESIAN_POINT ( 'NONE',  ( 0.000000000000000000, 0.000000000000000000, -1.239675197676287643 ) ) ;
#7547 = DIRECTION ( 'NONE',  ( 0.000000000000000000, 1.000000000000000000, 0.000000000000000000 ) ) ;
#7548 = CARTESIAN_POINT ( 'NONE',  ( -83.00000000000000000, 55.00000000000000711, -29.00000000000000355 ) ) ;
#7549 = CARTESIAN_POINT ( 'NONE',  ( -66.79270227826378914, 43.79499200241600931, 8.618888393567598172 ) ) ;
#7550 = ORIENTED_EDGE ( 'NONE', *, *, #4803, .T. ) ;
#7551 = FACE_OUTER_BOUND ( 'NONE', #6993, .T. ) ;
#7552 = AXIS2_PLACEMENT_3D ( 'NONE', #8565, #2207, #1243 ) ;
#7553 = CARTESIAN_POINT ( 'NONE',  ( -15.00000000000000000, 55.00000000000000000, 0.000000000000000000 ) ) ;
#7554 = CARTESIAN_POINT ( 'NONE',  ( -0.8179331680533127313, -5.301268757141564869, -0.1739375980333775218 ) ) ;
#7555 = LINE ( 'NONE', #3893, #6858 ) ;
#7556 = CARTESIAN_POINT ( 'NONE',  ( -8.153690333911775667, 67.55523279586272167, -21.62223061169231997 ) ) ;
#7557 = CARTESIAN_POINT ( 'NONE',  ( -79.34375000204839523, 55.00000000000000000, -25.81189881249999729 ) ) ;
#7558 = ORIENTED_EDGE ( 'NONE', *, *, #7197, .T. ) ;
#7559 = EDGE_CURVE ( 'NONE', #9652, #2004, #9587, .T. ) ;
#7560 = CARTESIAN_POINT ( 'NONE',  ( -78.31250000409679046, 72.67766952966368876, 17.67766952966368521 ) ) ;
#7561 = ORIENTED_EDGE ( 'NONE', *, *, #11121, .T. ) ;
#7562 = CARTESIAN_POINT ( 'NONE',  ( 9.245291525937640031, 68.12702208362456702, -21.27760407867818770 ) ) ;
#7563 = CARTESIAN_POINT ( 'NONE',  ( -62.74205264515926928, 46.08327288479434003, 10.86410523659212934 ) ) ;
#7564 = CARTESIAN_POINT ( 'NONE',  ( 14.99999999999999645, 0.000000000000000000, 30.00000000000000711 ) ) ;
#7565 = DIRECTION ( 'NONE',  ( -1.000000000000000000, -0.000000000000000000, -0.000000000000000000 ) ) ;
#7566 = EDGE_CURVE ( 'NONE', #7233, #9881, #2635, .T. ) ;
#7567 = EDGE_CURVE ( 'NONE', #8679, #9967, #8761, .T. ) ;
#7568 = CYLINDRICAL_SURFACE ( 'NONE', #2257, 2.500000000000000000 ) ;
#7569 = ORIENTED_EDGE ( 'NONE', *, *, #6412, .F. ) ;
#7570 = EDGE_CURVE ( 'NONE', #8673, #7792, #1929, .T. ) ;
#7571 = CARTESIAN_POINT ( 'NONE',  ( -71.37500000409677625, 55.00000000000000000, -24.99999999999999645 ) ) ;
#7572 = CARTESIAN_POINT ( 'NONE',  ( 46.99999999999999289, 58.53553390593273065, 3.535533905932731091 ) ) ;
#7573 = LINE ( 'NONE', #6961, #1521 ) ;
#7574 = CARTESIAN_POINT ( 'NONE',  ( -21.77654998131960795, 54.08371276951305617, 7.025374987337092314 ) ) ;
#7575 = PRODUCT_DEFINITION_FORMATION_WITH_SPECIFIED_SOURCE ( 'ANY', '', #2038, .NOT_KNOWN. ) ;
#7576 = AXIS2_PLACEMENT_3D ( 'NONE', #4773, #9440, #3995 ) ;
#7577 = CARTESIAN_POINT ( 'NONE',  ( -73.25000000000000000, 55.00000000000000000, 24.99999999999999645 ) ) ;
#7578 = DIRECTION ( 'NONE',  ( 0.000000000000000000, 0.000000000000000000, 1.000000000000000000 ) ) ;
#7579 = ORIENTED_EDGE ( 'NONE', *, *, #9671, .F. ) ;
#7580 = CARTESIAN_POINT ( 'NONE',  ( -78.00000000000001421, 63.48528137423857487, 8.485284746156350977 ) ) ;
#7581 = CARTESIAN_POINT ( 'NONE',  ( -78.00000000000001421, 46.51471862576140381, -8.485278002320759683 ) ) ;
#7582 = ORIENTED_EDGE ( 'NONE', *, *, #1525, .F. ) ;
#7583 = CARTESIAN_POINT ( 'NONE',  ( -36.14426256656389569, 36.63180902967581432, -10.58010824564746599 ) ) ;
#7584 = CARTESIAN_POINT ( 'NONE',  ( -75.40625000204839523, 36.74823131438026280, 18.25176868561974786 ) ) ;
#7585 = PLANE ( 'NONE',  #779 ) ;
#7586 = CARTESIAN_POINT ( 'NONE',  ( -80.00000000000000000, 55.00000000000000000, -24.99999999999999645 ) ) ;
#7587 = DIRECTION ( 'NONE',  ( 1.000000000000000000, 0.000000000000000000, 0.000000000000000000 ) ) ;
#7588 = ORIENTED_EDGE ( 'NONE', *, *, #4490, .F. ) ;
#7589 = CYLINDRICAL_SURFACE ( 'NONE', #8750, 1.500000000000000000 ) ;
#7590 = CARTESIAN_POINT ( 'NONE',  ( -10.04436138461520933, 58.30566320991975005, -3.765552063897302126 ) ) ;
#7591 = CARTESIAN_POINT ( 'NONE',  ( -80.00000000000002842, 50.75735931288069480, 12.72792543327563131 ) ) ;
#7592 = VECTOR ( 'NONE', #9430, 1000.000000000000000 ) ;
#7593 = VERTEX_POINT ( 'NONE', #997 ) ;
#7594 = CARTESIAN_POINT ( 'NONE',  ( 11.18907075893384828, 44.41926513478889404, 18.36970340340424457 ) ) ;
#7595 = CARTESIAN_POINT ( 'NONE',  ( 5.737947948793154396, 41.52763994192435604, 4.093911426704439194 ) ) ;
#7596 = CARTESIAN_POINT ( 'NONE',  ( 52.99999999999999289, 58.53553390593273065, 3.535533905932731091 ) ) ;
#7597 = FILL_AREA_STYLE_COLOUR ( '', #6049 ) ;
#7598 = DIRECTION ( 'NONE',  ( 1.000000000000000000, 0.000000000000000000, 0.000000000000000000 ) ) ;
#7599 = ORIENTED_EDGE ( 'NONE', *, *, #956, .T. ) ;
#7600 = EDGE_CURVE ( 'NONE', #1442, #3266, #10159, .T. ) ;
#7601 = CARTESIAN_POINT ( 'NONE',  ( -75.40625000000000000, 65.35533905932737753, -24.99999999999999645 ) ) ;
#7602 = CARTESIAN_POINT ( 'NONE',  ( 47.00000000000000000, 58.53553390593273065, -3.535533905932743526 ) ) ;
#7603 =( NAMED_UNIT ( * ) PLANE_ANGLE_UNIT ( ) SI_UNIT ( $, .RADIAN. ) );
#7604 = CIRCLE ( 'NONE', #506, 1.500000000000001332 ) ;
#7605 = DIRECTION ( 'NONE',  ( -1.000000000000000000, -0.000000000000000000, -0.000000000000000000 ) ) ;
#7606 = CARTESIAN_POINT ( 'NONE',  ( 1.916198795564182600, 48.29978761853648450, -2.032333837344214800 ) ) ;
#7607 = CIRCLE ( 'NONE', #1475, 1.500000000000001332 ) ;
#7608 = ORIENTED_EDGE ( 'NONE', *, *, #3901, .F. ) ;
#7609 = CARTESIAN_POINT ( 'NONE',  ( 3.697305843545918513, 35.98616635274733255, -8.992456113074794644 ) ) ;
#7610 = LINE ( 'NONE', #283, #1363 ) ;
#7611 = CARTESIAN_POINT ( 'NONE',  ( 52.99999999999999289, 55.00000000000000000, 0.000000000000000000 ) ) ;
#7612 = FACE_OUTER_BOUND ( 'NONE', #9637, .T. ) ;
#7613 = CARTESIAN_POINT ( 'NONE',  ( -24.87631665557734095, 79.64556585907233455, -4.276919348231523976 ) ) ;
#7614 = CARTESIAN_POINT ( 'NONE',  ( -78.68750000204839523, 65.69163855873949842, 25.81189881250000440 ) ) ;
#7615 = ORIENTED_EDGE ( 'NONE', *, *, #7825, .T. ) ;
#7616 = AXIS2_PLACEMENT_3D ( 'NONE', #372, #4037, #3914 ) ;
#7617 = CARTESIAN_POINT ( 'NONE',  ( -71.75000000204840944, 65.69163855873948421, -25.81189881250000440 ) ) ;
#7618 = FACE_BOUND ( 'NONE', #6115, .T. ) ;
#7619 = CARTESIAN_POINT ( 'NONE',  ( 24.23505289248274863, 79.09914288581300923, -6.663429661133934978 ) ) ;
#7620 = CARTESIAN_POINT ( 'NONE',  ( 19.52230480204648799, 67.92440004991483704, 16.80766691833610693 ) ) ;
#7621 = CYLINDRICAL_SURFACE ( 'NONE', #2321, 2.500000000000000000 ) ;
#7622 = CARTESIAN_POINT ( 'NONE',  ( -75.00000000000000000, 80.20344453945780572, -1.438425885725281628 ) ) ;
#7623 = DIRECTION ( 'NONE',  ( -1.000000000000000000, -0.000000000000000000, -0.000000000000000000 ) ) ;
#7624 = VECTOR ( 'NONE', #2343, 1000.000000000000000 ) ;
#7625 = EDGE_LOOP ( 'NONE', ( #6154, #10894, #5544, #7342, #526 ) ) ;
#7626 = CARTESIAN_POINT ( 'NONE',  ( -77.56250000000000000, 37.32233047033631124, 17.67766952966369232 ) ) ;
#7627 = CYLINDRICAL_SURFACE ( 'NONE', #9940, 2.500000000000000000 ) ;
#7628 = CARTESIAN_POINT ( 'NONE',  ( -43.29000404689811177, 55.16495308597901470, -4.999994068545482229 ) ) ;
#7629 = EDGE_LOOP ( 'NONE', ( #10367, #341 ) ) ;
#7630 = EDGE_CURVE ( 'NONE', #5363, #3229, #5625, .T. ) ;
#7631 = CARTESIAN_POINT ( 'NONE',  ( 24.88735338357604476, 62.02547980208617417, 0.9195476851153630005 ) ) ;
#7632 = CARTESIAN_POINT ( 'NONE',  ( -12.32394926038158012, 69.76387561330639642, 16.31736050817429984 ) ) ;
#7633 = CARTESIAN_POINT ( 'NONE',  ( 47.00000000000000711, 51.46446609406725514, 3.535533905932731091 ) ) ;
#7634 = ORIENTED_EDGE ( 'NONE', *, *, #1959, .T. ) ;
#7635 = CARTESIAN_POINT ( 'NONE',  ( -4.999999999999999112, -2.417244626924487605, -5.788952927922133007 ) ) ;
#7636 = CARTESIAN_POINT ( 'NONE',  ( -78.03125000204838102, 55.00000000000000000, -25.81189881249999729 ) ) ;
#7637 = EDGE_CURVE ( 'NONE', #6597, #11278, #10149, .T. ) ;
#7638 = CONICAL_SURFACE ( 'NONE', #5923, 5.000000000000000888, 1.047197551196596299 ) ;
#7639 = ORIENTED_EDGE ( 'NONE', *, *, #4379, .F. ) ;
#7640 = CARTESIAN_POINT ( 'NONE',  ( -33.30269350532120143, 33.99387206627966407, -1.031609878214063025 ) ) ;
#7641 = CARTESIAN_POINT ( 'NONE',  ( -73.43750000204839523, 44.30836144126050158, -25.81189881249999374 ) ) ;
#7642 = CARTESIAN_POINT ( 'NONE',  ( -76.43750000000005684, 72.67766952966361771, 17.67766952966361771 ) ) ;
#7643 = CARTESIAN_POINT ( 'NONE',  ( -53.73751484135783585, 71.24472392590685388, 13.33357819947211453 ) ) ;
#7644 =( NAMED_UNIT ( * ) PLANE_ANGLE_UNIT ( ) SI_UNIT ( $, .RADIAN. ) );
#7645 = AXIS2_PLACEMENT_3D ( 'NONE', #10703, #645, #4306 ) ;
#7646 = CARTESIAN_POINT ( 'NONE',  ( -77.46875000409679046, 44.64466094067266511, -25.00000000000004263 ) ) ;
#7647 = ORIENTED_EDGE ( 'NONE', *, *, #5286, .F. ) ;
#7648 = DIRECTION ( 'NONE',  ( 0.000000000000000000, 0.000000000000000000, 1.000000000000000000 ) ) ;
#7649 = CARTESIAN_POINT ( 'NONE',  ( -7.320490228006724998, 56.29691533456504970, -4.839845655098152122 ) ) ;
#7650 = CARTESIAN_POINT ( 'NONE',  ( 10.52240409369262153, 44.41989175727180594, 18.36819097564579195 ) ) ;
#7651 = EDGE_LOOP ( 'NONE', ( #10816, #420, #10108, #6369 ) ) ;
#7652 = CARTESIAN_POINT ( 'NONE',  ( 6.725052486299625265, 34.79623650017382630, 6.139562429837428503 ) ) ;
#7653 = CARTESIAN_POINT ( 'NONE',  ( -61.88037028687247698, 51.91449295574040690, 20.80032498971814192 ) ) ;
#7654 = CARTESIAN_POINT ( 'NONE',  ( -78.68750000000002842, 37.32233047033633966, -17.67766952966366034 ) ) ;
#7655 = DIRECTION ( 'NONE',  ( 0.000000000000000000, 0.000000000000000000, 1.000000000000000000 ) ) ;
#7656 = CIRCLE ( 'NONE', #7274, 4.999999999999990230 ) ;
#7657 = DIRECTION ( 'NONE',  ( -1.000000000000000000, -0.000000000000000000, -0.000000000000000000 ) ) ;
#7658 = ORIENTED_EDGE ( 'NONE', *, *, #8437, .F. ) ;
#7659 = EDGE_CURVE ( 'NONE', #9917, #7121, #5502, .T. ) ;
#7660 = CARTESIAN_POINT ( 'NONE',  ( -77.46875000000000000, 30.00000000000001421, 10.35533905932739174 ) ) ;
#7661 = LINE ( 'NONE', #398, #9285 ) ;
#7662 = SURFACE_STYLE_USAGE ( .BOTH. , #2015 ) ;
#7663 = CIRCLE ( 'NONE', #2485, 1.500000000000001332 ) ;
#7664 = CARTESIAN_POINT ( 'NONE',  ( 39.99999999999999289, 55.00000000000000000, 0.000000000000000000 ) ) ;
#7665 = CARTESIAN_POINT ( 'NONE',  ( -7.708699213456044141, 57.35874996863078934, -6.593436642072879827 ) ) ;
#7666 = EDGE_LOOP ( 'NONE', ( #2979, #11069, #2949, #6352 ) ) ;
#7667 = CARTESIAN_POINT ( 'NONE',  ( -40.33720992201957500, 55.00042869323097960, -21.02810349118288258 ) ) ;
#7668 = CYLINDRICAL_SURFACE ( 'NONE', #9770, 1.499999999999999556 ) ;
#7669 = LINE ( 'NONE', #3225, #9832 ) ;
#7670 = CARTESIAN_POINT ( 'NONE',  ( -75.21875000204839523, 29.18810118750000271, 4.741568889096522788E-15 ) ) ;
#7671 = CARTESIAN_POINT ( 'NONE',  ( 52.99999999999999289, 55.00000000000000000, -3.000000000000002665 ) ) ;
#7672 = CARTESIAN_POINT ( 'NONE',  ( -71.93750000204838102, 65.69163855873948421, -25.81189881250000440 ) ) ;
#7673 = VERTEX_POINT ( 'NONE', #31 ) ;
#7674 = CARTESIAN_POINT ( 'NONE',  ( -77.28125000409677625, 65.35533905932737753, -24.99999999999999645 ) ) ;
#7675 = FACE_BOUND ( 'NONE', #2916, .T. ) ;
#7676 = CARTESIAN_POINT ( 'NONE',  ( 16.74161068948953357, 73.05576634196897601, -17.30319104633145955 ) ) ;
#7677 = CARTESIAN_POINT ( 'NONE',  ( -45.46040646759425385, 66.21151220796895132, -8.622207064378679675 ) ) ;
#7678 = EDGE_CURVE ( 'NONE', #8851, #1911, #5774, .T. ) ;
#7679 = CARTESIAN_POINT ( 'NONE',  ( -78.59375000204839523, 36.74823131438026280, 18.25176868561974786 ) ) ;
#7680 = FACE_OUTER_BOUND ( 'NONE', #6627, .T. ) ;
#7681 = AXIS2_PLACEMENT_3D ( 'NONE', #10290, #11120, #8503 ) ;
#7682 = FACE_OUTER_BOUND ( 'NONE', #8116, .T. ) ;
#7683 = VERTEX_POINT ( 'NONE', #6294 ) ;
#7684 = CARTESIAN_POINT ( 'NONE',  ( -74.18750000000000000, 37.32233047033631124, -17.67766952966368166 ) ) ;
#7685 = LINE ( 'NONE', #11375, #10322 ) ;
#7686 = CARTESIAN_POINT ( 'NONE',  ( -41.54352521660307929, 53.70653700278867859, -4.840732458542600369 ) ) ;
#7687 = ORIENTED_EDGE ( 'NONE', *, *, #8705, .T. ) ;
#7688 = EDGE_CURVE ( 'NONE', #3207, #6726, #9925, .T. ) ;
#7689 = CARTESIAN_POINT ( 'NONE',  ( 14.77655085292736281, 53.17745613723639053, 6.794376823515287711 ) ) ;
#7690 = CARTESIAN_POINT ( 'NONE',  ( 0.000000000000000000, 0.000000000000000000, 0.000000000000000000 ) ) ;
#7691 = AXIS2_PLACEMENT_3D ( 'NONE', #8093, #4659, #4489 ) ;
#7692 = FILL_AREA_STYLE_COLOUR ( '', #3001 ) ;
#7693 = CIRCLE ( 'NONE', #3866, 1.500000000000001332 ) ;
#7694 = ORIENTED_EDGE ( 'NONE', *, *, #10219, .F. ) ;
#7695 = CARTESIAN_POINT ( 'NONE',  ( 34.00000000000000000, 55.00000000000000000, 0.000000000000000000 ) ) ;
#7696 = CARTESIAN_POINT ( 'NONE',  ( -78.59375000204839523, 36.74823131438026280, 18.25176868561974786 ) ) ;
#7697 = EDGE_LOOP ( 'NONE', ( #5879, #2114 ) ) ;
#7698 = CARTESIAN_POINT ( 'NONE',  ( -65.06671514604981610, 41.61929618219224380, 16.30332023460171698 ) ) ;
#7699 = CARTESIAN_POINT ( 'NONE',  ( -71.40810441781462714, 80.81189881250000440, 6.916273779317701376 ) ) ;
#7700 = EDGE_CURVE ( 'NONE', #6451, #6801, #8057, .T. ) ;
#7701 = EDGE_CURVE ( 'NONE', #10478, #884, #4656, .T. ) ;
#7702 = EDGE_CURVE ( 'NONE', #8432, #3359, #5971, .T. ) ;
#7703 = CARTESIAN_POINT ( 'NONE',  ( -75.68750000409677625, 72.67766952966368876, -17.67766952966368876 ) ) ;
#7704 = CARTESIAN_POINT ( 'NONE',  ( -57.82750524721426189, 59.10997802641301035, 20.69196764327204008 ) ) ;
#7705 = DIRECTION ( 'NONE',  ( -1.000000000000000000, 0.000000000000000000, 0.000000000000000000 ) ) ;
#7706 = ORIENTED_EDGE ( 'NONE', *, *, #9937, .F. ) ;
#7707 = CARTESIAN_POINT ( 'NONE',  ( -78.00000000000001421, 50.75735931288069480, -14.22791868944003646 ) ) ;
#7708 = CARTESIAN_POINT ( 'NONE',  ( -2.500000000000003553, 4.330127018922192761, 0.000000000000000000 ) ) ;
#7709 = B_SPLINE_CURVE_WITH_KNOTS ( 'NONE', 3,
 ( #6365, #7319, #8148, #5512, #3533, #9823, #882, #11672, #10830, #943, #7147, #10946, #3595, #8206, #11842, #1844, #10770, #2582, #4610, #8265, #40, #2524, #6248, #6190, #1612, #9875, #1671, #5339, #8991, #5573, #1007, #8506, #9219, #4667 ),
 .UNSPECIFIED., .F., .F.,
 ( 4, 2, 2, 2, 2, 2, 2, 2, 2, 2, 2, 2, 2, 2, 2, 2, 4 ),
 ( 0.000000000000000000, 0.001517779093106276078, 0.003035558186212552155, 0.004553337279318827799, 0.006071116372425104310, 0.007588895465531380821, 0.009106674558637655598, 0.01062445365174393211, 0.01214223274485020862, 0.01366001183795648513, 0.01517779093106276164, 0.01669557002416903815, 0.01821334911727531120, 0.01973112821038158771, 0.02124890730348786422, 0.02276668639659414073, 0.02428446548970041724 ),
 .UNSPECIFIED. ) ;
#7710 = ADVANCED_FACE ( 'NONE', ( #8309, #1055 ), #2194, .F. ) ;
#7711 = CARTESIAN_POINT ( 'NONE',  ( -20.73741325422386339, 64.90628579765783002, 18.53688757488948369 ) ) ;
#7712 = ADVANCED_FACE ( 'NONE', ( #10280 ), #3864, .T. ) ;
#7713 = VERTEX_POINT ( 'NONE', #1762 ) ;
#7714 = CARTESIAN_POINT ( 'NONE',  ( -65.84115524907865336, 36.67226210568770028, 10.55087792480968112 ) ) ;
#7715 = CARTESIAN_POINT ( 'NONE',  ( -32.45530648322815637, 41.13881078342074460, 2.056777965717148327 ) ) ;
#7716 = DIRECTION ( 'NONE',  ( 0.000000000000000000, 0.000000000000000000, 1.000000000000000000 ) ) ;
#7717 = CARTESIAN_POINT ( 'NONE',  ( -78.00000000000002842, 46.51471862576140381, -1.499996628082201244 ) ) ;
#7718 = EDGE_CURVE ( 'NONE', #7495, #2377, #11189, .T. ) ;
#7719 = UNCERTAINTY_MEASURE_WITH_UNIT (LENGTH_MEASURE( 1.000000000000000082E-05 ), #5301, 'distance_accuracy_value', 'NONE');
#7720 = CYLINDRICAL_SURFACE ( 'NONE', #3436, 25.00000000000000355 ) ;
#7721 = ORIENTED_EDGE ( 'NONE', *, *, #10757, .F. ) ;
#7722 = CARTESIAN_POINT ( 'NONE',  ( -75.59375000000000000, 44.64466094067260826, -24.99999999999998934 ) ) ;
#7723 = DIRECTION ( 'NONE',  ( -1.000000000000000000, -0.000000000000000000, -0.000000000000000000 ) ) ;
#7724 = DIRECTION ( 'NONE',  ( 0.000000000000000000, 1.000000000000000000, 0.000000000000000000 ) ) ;
#7725 = CARTESIAN_POINT ( 'NONE',  ( -34.83316205860364079, 48.09832289792718285, -1.369967489524484883 ) ) ;
#7726 = VERTEX_POINT ( 'NONE', #2061 ) ;
#7727 = CARTESIAN_POINT ( 'NONE',  ( -31.30269415623623885, 33.99224428815358579, -1.031667027462585207 ) ) ;
#7728 = LINE ( 'NONE', #2021, #11766 ) ;
#7729 = CARTESIAN_POINT ( 'NONE',  ( 14.99999999999999645, 0.000000000000000000, 30.00000000000000711 ) ) ;
#7730 = CARTESIAN_POINT ( 'NONE',  ( -74.93750000204838102, 44.30836144126049447, -25.81189881249999019 ) ) ;
#7731 = CARTESIAN_POINT ( 'NONE',  ( -24.88738022673829775, 79.65503066217630135, 4.221719104015677182 ) ) ;
#7732 = CARTESIAN_POINT ( 'NONE',  ( -73.81250000204839523, 29.18810118750000626, -10.69163855873949309 ) ) ;
#7733 = ORIENTED_EDGE ( 'NONE', *, *, #8135, .F. ) ;
#7734 = CARTESIAN_POINT ( 'NONE',  ( -76.62500000409677625, 55.00000000000000000, 24.99999999999999645 ) ) ;
#7735 = CARTESIAN_POINT ( 'NONE',  ( -80.00000000000002842, 50.75735931288069480, 2.742644059037076865 ) ) ;
#7736 = CARTESIAN_POINT ( 'NONE',  ( 0.000000000000000000, 0.000000000000000000, 0.000000000000000000 ) ) ;
#7737 = CARTESIAN_POINT ( 'NONE',  ( -21.05849041552747281, 57.05917194494736577, 20.98221040122819403 ) ) ;
#7738 = CARTESIAN_POINT ( 'NONE',  ( -78.12500000204839523, 44.30836144126049447, -25.81189881249999019 ) ) ;
#7739 = AXIS2_PLACEMENT_3D ( 'NONE', #3168, #7784, #8447 ) ;
#7740 = CARTESIAN_POINT ( 'NONE',  ( -75.00000000000000000, 55.00000000000000000, 0.000000000000000000 ) ) ;
#7741 = CARTESIAN_POINT ( 'NONE',  ( -73.53125000000005684, 79.99999999999987210, 10.35533905932731891 ) ) ;
#7742 = EDGE_LOOP ( 'NONE', ( #7588, #2166, #8203, #2170 ) ) ;
#7743 = CARTESIAN_POINT ( 'NONE',  ( -76.53124999999998579, 80.00000000000001421, 10.35533905932737397 ) ) ;
#7744 = CARTESIAN_POINT ( 'NONE',  ( -71.00000000409677625, 80.00000000000000000, -1.530808498934191324E-15 ) ) ;
#7745 = CYLINDRICAL_SURFACE ( 'NONE', #4233, 25.00000000000000355 ) ;
#7746 = ORIENTED_EDGE ( 'NONE', *, *, #140, .T. ) ;
#7747 = CARTESIAN_POINT ( 'NONE',  ( -34.22341864884656104, 49.42024689336786736, -4.283880285341411742 ) ) ;
#7748 = CARTESIAN_POINT ( 'NONE',  ( -3.970850827666276395, 65.56567621485199027, 19.29717822822915707 ) ) ;
#7749 = VERTEX_POINT ( 'NONE', #4947 ) ;
#7750 = CARTESIAN_POINT ( 'NONE',  ( 7.008258234807173359, 66.69771099951718440, 18.63519012541959441 ) ) ;
#7751 = CARTESIAN_POINT ( 'NONE',  ( -2.074714256722480332, 4.575665857285978966, -6.089444439476609183 ) ) ;
#7752 = ORIENTED_EDGE ( 'NONE', *, *, #3418, .T. ) ;
#7753 = CARTESIAN_POINT ( 'NONE',  ( 62.44550000000000267, 55.00000000000000000, 2.999999999999995559 ) ) ;
#7754 =( GEOMETRIC_REPRESENTATION_CONTEXT ( 3 ) GLOBAL_UNCERTAINTY_ASSIGNED_CONTEXT ( ( #11289 ) ) GLOBAL_UNIT_ASSIGNED_CONTEXT ( ( #5611, #10140, #1038 ) ) REPRESENTATION_CONTEXT ( 'NONE', 'WORKASPACE' ) );
#7755 = AXIS2_PLACEMENT_3D ( 'NONE', #5743, #3878, #7655 ) ;
#7756 = DIRECTION ( 'NONE',  ( -1.000000000000000000, 0.000000000000000000, 0.000000000000000000 ) ) ;
#7757 = CARTESIAN_POINT ( 'NONE',  ( -78.87500000409677625, 55.00000000000000000, -24.99999999999999645 ) ) ;
#7758 = DIRECTION ( 'NONE',  ( -0.9999998346844721775, 0.0005712585774195265247, -6.553370117834432030E-05 ) ) ;
#7759 = ORIENTED_EDGE ( 'NONE', *, *, #10730, .F. ) ;
#7760 = B_SPLINE_CURVE_WITH_KNOTS ( 'NONE', 3,
 ( #2872, #9777, #1573, #5238, #8885, #3427 ),
 .UNSPECIFIED., .F., .F.,
 ( 4, 2, 4 ),
 ( 0.008070708573309215428, 0.009531758523483287518, 0.01099280847365735961 ),
 .UNSPECIFIED. ) ;
#7761 = CYLINDRICAL_SURFACE ( 'NONE', #1666, 1.499999999999999556 ) ;
#7762 = CARTESIAN_POINT ( 'NONE',  ( -24.47759590008010377, 52.25445690686086664, 21.01882782503509262 ) ) ;
#7763 = VERTEX_POINT ( 'NONE', #3920 ) ;
#7764 = CARTESIAN_POINT ( 'NONE',  ( -12.85572911067665380, 75.97954889423452585, -2.745668038893096519 ) ) ;
#7765 = CARTESIAN_POINT ( 'NONE',  ( -42.66853512798572012, 55.00035148751268110, -14.01901578153819727 ) ) ;
#7766 = LINE ( 'NONE', #4167, #6508 ) ;
#7767 = CARTESIAN_POINT ( 'NONE',  ( -80.00000000000002842, 50.75735931288069480, 14.22792543327563131 ) ) ;
#7768 = PRODUCT ( 'MAS-170', 'MAS-170', '', ( #6564 ) ) ;
#7769 = AXIS2_PLACEMENT_3D ( 'NONE', #3890, #11175, #5874 ) ;
#7770 = CARTESIAN_POINT ( 'NONE',  ( -17.04105779988202585, 59.74509268894269098, 1.609841060220320141 ) ) ;
#7771 = ORIENTED_EDGE ( 'NONE', *, *, #10482, .F. ) ;
#7772 = CARTESIAN_POINT ( 'NONE',  ( -74.37500000000000000, 30.00000000000000355, 4.592425496802573578E-15 ) ) ;
#7773 = CARTESIAN_POINT ( 'NONE',  ( -75.00000000000000000, 40.74342228783053343, -21.53420582633694025 ) ) ;
#7774 = EDGE_CURVE ( 'NONE', #5996, #7952, #2312, .T. ) ;
#7775 = FILL_AREA_STYLE ('',( #11466 ) ) ;
#7776 = VECTOR ( 'NONE', #5934, 1000.000000000000000 ) ;
#7777 = FACE_OUTER_BOUND ( 'NONE', #2234, .T. ) ;
#7778 = CARTESIAN_POINT ( 'NONE',  ( -21.12525410080779054, 58.60173025390926682, 6.007737297149077449 ) ) ;
#7779 = ORIENTED_EDGE ( 'NONE', *, *, #2839, .F. ) ;
#7780 = CARTESIAN_POINT ( 'NONE',  ( -48.14429339001110009, 75.47411806927735256, -5.508782930744743567 ) ) ;
#7781 = VECTOR ( 'NONE', #4035, 1000.000000000000114 ) ;
#7782 = EDGE_CURVE ( 'NONE', #8790, #3229, #9593, .T. ) ;
#7783 = DIRECTION ( 'NONE',  ( -0.000000000000000000, -0.000000000000000000, -1.000000000000000000 ) ) ;
#7784 = DIRECTION ( 'NONE',  ( 0.000000000000000000, 0.000000000000000000, 1.000000000000000000 ) ) ;
#7785 = EDGE_CURVE ( 'NONE', #6797, #30, #4828, .T. ) ;
#7786 = CARTESIAN_POINT ( 'NONE',  ( -76.06250000204842365, 80.81189881250000440, -10.69163855873948954 ) ) ;
#7787 = CARTESIAN_POINT ( 'NONE',  ( -20.69108674001310177, 76.15158908439804009, 13.33178032960098314 ) ) ;
#7788 = CARTESIAN_POINT ( 'NONE',  ( -74.00000000204840944, 44.30836144126053000, 25.81189881250000795 ) ) ;
#7789 = EDGE_LOOP ( 'NONE', ( #8488, #1909, #2297, #9453 ) ) ;
#7790 = DIRECTION ( 'NONE',  ( -1.000000000000000000, -0.000000000000000000, -0.000000000000000000 ) ) ;
#7791 = CARTESIAN_POINT ( 'NONE',  ( -78.00000000000000000, 54.99999999999999289, 0.000000000000000000 ) ) ;
#7792 = VERTEX_POINT ( 'NONE', #5795 ) ;
#7793 = CARTESIAN_POINT ( 'NONE',  ( -10.81092923698156838, 75.47407628921179423, -5.508885182882011122 ) ) ;
#7794 = AXIS2_PLACEMENT_3D ( 'NONE', #9056, #2648, #1622 ) ;
#7795 = CARTESIAN_POINT ( 'NONE',  ( -77.18750000204838102, 44.30836144126052289, 25.81189881250000795 ) ) ;
#7796 = CARTESIAN_POINT ( 'NONE',  ( -78.00000000000002842, 54.99999999999998579, 16.97056612039490986 ) ) ;
#7797 = DIRECTION ( 'NONE',  ( -1.000000000000000000, 0.000000000000000000, 0.000000000000000000 ) ) ;
#7798 = VERTEX_POINT ( 'NONE', #135 ) ;
#7799 = CARTESIAN_POINT ( 'NONE',  ( 14.99999999999999645, 5.000000000000000000, -29.99999999999999289 ) ) ;
#7800 = VECTOR ( 'NONE', #11299, 1000.000000000000000 ) ;
#7801 = CARTESIAN_POINT ( 'NONE',  ( -75.68750000000000000, 37.32233047033631124, -17.67766952966368166 ) ) ;
#7802 = CARTESIAN_POINT ( 'NONE',  ( -78.00000000000002842, 38.02943725152282184, -1.499996628082202133 ) ) ;
#7803 = CARTESIAN_POINT ( 'NONE',  ( -50.87777401005003242, 59.84064543832867855, -1.293741243580276645 ) ) ;
#7804 = ORIENTED_EDGE ( 'NONE', *, *, #3458, .F. ) ;
#7805 = EDGE_CURVE ( 'NONE', #2575, #4892, #9307, .T. ) ;
#7806 = CARTESIAN_POINT ( 'NONE',  ( -51.91627845054419765, 61.18957700299936420, 3.307427248076153070 ) ) ;
#7807 = CARTESIAN_POINT ( 'NONE',  ( -77.46875000000005684, 30.00000000000010303, 10.35533905932735443 ) ) ;
#7808 = SURFACE_STYLE_FILL_AREA ( #10487 ) ;
#7809 = CIRCLE ( 'NONE', #8965, 25.00000000000000355 ) ;
#7810 = ORIENTED_EDGE ( 'NONE', *, *, #4675, .F. ) ;
#7811 = CARTESIAN_POINT ( 'NONE',  ( 21.36911699583331270, 76.71007065292897664, -3.630805090811919378 ) ) ;
#7812 = CARTESIAN_POINT ( 'NONE',  ( -0.8192951148925881055, 5.300482436767277150, -5.901655677627839935 ) ) ;
#7813 = VERTEX_POINT ( 'NONE', #9427 ) ;
#7814 = CARTESIAN_POINT ( 'NONE',  ( -76.06250000204840944, 80.81189881250001861, -10.69163855873949132 ) ) ;
#7815 = VECTOR ( 'NONE', #4315, 1000.000000000000000 ) ;
#7816 = DIRECTION ( 'NONE',  ( -1.000000000000000000, -0.000000000000000000, -0.000000000000000000 ) ) ;
#7817 = CARTESIAN_POINT ( 'NONE',  ( -14.83686862936316331, 54.99606387762347026, -0.004311921550151643669 ) ) ;
#7818 =( NAMED_UNIT ( * ) SI_UNIT ( $, .STERADIAN. ) SOLID_ANGLE_UNIT ( ) );
#7819 = LINE ( 'NONE', #321, #310 ) ;
#7820 = ADVANCED_FACE ( 'NONE', ( #1940 ), #5977, .F. ) ;
#7821 = ORIENTED_EDGE ( 'NONE', *, *, #4702, .T. ) ;
#7822 = DIRECTION ( 'NONE',  ( 0.000000000000000000, 0.000000000000000000, 1.000000000000000000 ) ) ;
#7823 = CARTESIAN_POINT ( 'NONE',  ( -46.39182477221876866, 68.38321102182860045, -16.29532114285349920 ) ) ;
#7824 = EDGE_LOOP ( 'NONE', ( #1883, #1138, #9985, #6018 ) ) ;
#7825 = EDGE_CURVE ( 'NONE', #723, #4662, #3855, .T. ) ;
#7826 = CARTESIAN_POINT ( 'NONE',  ( 17.47768387407981905, 65.56544091938442875, 18.33174872895543928 ) ) ;
#7827 = CARTESIAN_POINT ( 'NONE',  ( -8.544800298261920446, 62.20752307867830666, -12.02527808387988806 ) ) ;
#7828 = PLANE ( 'NONE',  #9180 ) ;
#7829 = CARTESIAN_POINT ( 'NONE',  ( -76.43750000409679046, 37.32233047033631124, 17.67766952966369232 ) ) ;
#7830 = CARTESIAN_POINT ( 'NONE',  ( -20.15075984075561522, 58.30274989043048350, 3.768099053302629731 ) ) ;
#7831 = VECTOR ( 'NONE', #4849, 1000.000000000000000 ) ;
#7832 = VERTEX_POINT ( 'NONE', #8535 ) ;
#7833 = CARTESIAN_POINT ( 'NONE',  ( -72.40625000000000000, 65.35533905932737753, -24.99999999999999645 ) ) ;
#7834 = DIRECTION ( 'NONE',  ( 0.8191520442889974607, 1.003171929053531649E-16, -0.5735764363510379438 ) ) ;
#7835 = EDGE_CURVE ( 'NONE', #1507, #11839, #9986, .T. ) ;
#7836 = CARTESIAN_POINT ( 'NONE',  ( -80.00000000000001421, 63.48528137423857487, 1.500003371917795425 ) ) ;
#7837 = VECTOR ( 'NONE', #242, 1000.000000000000000 ) ;
#7838 = CARTESIAN_POINT ( 'NONE',  ( -80.00000000000001421, 50.75735931288069480, -12.72791868944003824 ) ) ;
#7839 = CARTESIAN_POINT ( 'NONE',  ( -51.55667834818763851, 61.98283010711340779, -0.9164068158849860701 ) ) ;
#7840 = CIRCLE ( 'NONE', #5535, 21.50000000000000000 ) ;
#7841 = ORIENTED_EDGE ( 'NONE', *, *, #9045, .F. ) ;
#7842 = CARTESIAN_POINT ( 'NONE',  ( -55.50627899214600092, 66.73177265193905328, 17.54361557889675893 ) ) ;
#7843 = CARTESIAN_POINT ( 'NONE',  ( 10.52240409369262153, 44.41989175727180594, 18.36819097564579195 ) ) ;
#7844 = ADVANCED_FACE ( 'NONE', ( #11274 ), #3085, .F. ) ;
#7845 = CARTESIAN_POINT ( 'NONE',  ( 9.999999999999994671, 0.000000000000000000, -10.00000000000000000 ) ) ;
#7846 = CARTESIAN_POINT ( 'NONE',  ( -74.84375000204839523, 55.00000000000000000, -25.81189881249999729 ) ) ;
#7847 = CARTESIAN_POINT ( 'NONE',  ( -16.74856700446162705, 73.06100190697902974, 17.29768990044683363 ) ) ;
#7848 = CARTESIAN_POINT ( 'NONE',  ( -73.53125000204839523, 36.74823131438024859, -18.25176868561973720 ) ) ;
#7849 = ORIENTED_EDGE ( 'NONE', *, *, #7125, .T. ) ;
#7850 = CARTESIAN_POINT ( 'NONE',  ( -72.59375000409677625, 80.00000000000001421, -10.35533905932737753 ) ) ;
#7851 = FACE_BOUND ( 'NONE', #3471, .T. ) ;
#7852 = EDGE_LOOP ( 'NONE', ( #10432, #1944, #2715, #225, #4477 ) ) ;
#7853 = VECTOR ( 'NONE', #11460, 1000.000000000000000 ) ;
#7854 = CARTESIAN_POINT ( 'NONE',  ( -13.85565285731654761, 75.43037139504293975, 5.490367781071763709 ) ) ;
#7855 = CARTESIAN_POINT ( 'NONE',  ( -75.03125000000005684, 79.99999999999990052, 10.35533905932732779 ) ) ;
#7856 = DIRECTION ( 'NONE',  ( 0.000000000000000000, 0.000000000000000000, -1.000000000000000000 ) ) ;
#7857 = ADVANCED_BREP_SHAPE_REPRESENTATION ( '', ( #912, #4738 ), #3395 ) ;
#7858 = CARTESIAN_POINT ( 'NONE',  ( 0.000000000000000000, 0.000000000000000000, 0.000000000000000000 ) ) ;
#7859 = ORIENTED_EDGE ( 'NONE', *, *, #7702, .T. ) ;
#7860 = DIRECTION ( 'NONE',  ( -1.000000000000000000, -0.000000000000000000, -0.000000000000000000 ) ) ;
#7861 = CARTESIAN_POINT ( 'NONE',  ( -74.93750000000000000, 72.67766952966368876, 17.67766952966368521 ) ) ;
#7862 = CARTESIAN_POINT ( 'NONE',  ( -78.00000000000001421, 71.97056274847716395, 1.500003371917795425 ) ) ;
#7863 = ADVANCED_FACE ( 'NONE', ( #6754, #4045 ), #7585, .T. ) ;
#7864 = FACE_OUTER_BOUND ( 'NONE', #8727, .T. ) ;
#7865 = AXIS2_PLACEMENT_3D ( 'NONE', #9323, #10558, #11446 ) ;
#7866 = PRODUCT_DEFINITION_CONTEXT ( 'detailed design', #2255, 'design' ) ;
#7867 = ORIENTED_EDGE ( 'NONE', *, *, #4051, .T. ) ;
#7868 = CARTESIAN_POINT ( 'NONE',  ( -33.44321664797443105, 48.86004778347864885, -3.535033631877461335 ) ) ;
#7869 = AXIS2_PLACEMENT_3D ( 'NONE', #1701, #6386, #6626 ) ;
#7870 = CARTESIAN_POINT ( 'NONE',  ( -77.37500000000005684, 30.00000000000009592, 4.592425496802557801E-15 ) ) ;
#7871 = LINE ( 'NONE', #3312, #7781 ) ;
#7872 = ORIENTED_EDGE ( 'NONE', *, *, #2288, .T. ) ;
#7873 = DIRECTION ( 'NONE',  ( 0.000000000000000000, 1.000000000000000000, 0.000000000000000000 ) ) ;
#7874 = AXIS2_PLACEMENT_3D ( 'NONE', #11832, #7309, #9149 ) ;
#7875 = AXIS2_PLACEMENT_3D ( 'NONE', #7097, #10779, #9228 ) ;
#7876 = CARTESIAN_POINT ( 'NONE',  ( -77.56250000204838102, 80.81189881250000440, 10.69163855873948243 ) ) ;
#7877 = ORIENTED_EDGE ( 'NONE', *, *, #1332, .T. ) ;
#7878 = CARTESIAN_POINT ( 'NONE',  ( -78.59375000204839523, 55.00000000000000000, 25.81189881249999729 ) ) ;
#7879 = CARTESIAN_POINT ( 'NONE',  ( 0.000000000000000000, 0.000000000000000000, -6.099999999999999645 ) ) ;
#7880 = CARTESIAN_POINT ( 'NONE',  ( -75.78125000409680467, 65.35533905932749121, -24.99999999999989342 ) ) ;
#7881 = CARTESIAN_POINT ( 'NONE',  ( -9.759360353501660867, 55.02483400675389902, -0.008490801778254833052 ) ) ;
#7882 = CIRCLE ( 'NONE', #5202, 1.500000000000001332 ) ;
#7883 = VECTOR ( 'NONE', #7860, 1000.000000000000000 ) ;
#7884 = DIRECTION ( 'NONE',  ( 0.000000000000000000, 0.000000000000000000, 1.000000000000000000 ) ) ;
#7885 = ORIENTED_EDGE ( 'NONE', *, *, #10019, .F. ) ;
#7886 = CARTESIAN_POINT ( 'NONE',  ( -3.556264818047240706, -3.720292241887095397, -0.08165819712377302142 ) ) ;
#7887 = CARTESIAN_POINT ( 'NONE',  ( -28.94161417925737823, 38.68453375511723635, 13.40299329694203578 ) ) ;
#7888 = ORIENTED_EDGE ( 'NONE', *, *, #8182, .T. ) ;
#7889 = CARTESIAN_POINT ( 'NONE',  ( -61.78348097019890162, 49.89195498129476647, 20.38977643156359676 ) ) ;
#7890 = CARTESIAN_POINT ( 'NONE',  ( -8.256150493756077680, 61.60926336870365105, -12.36828619365871695 ) ) ;
#7891 = VECTOR ( 'NONE', #2978, 1000.000000000000000 ) ;
#7892 = CARTESIAN_POINT ( 'NONE',  ( -74.56250000204839523, 80.81189881250001861, 10.69163855873948599 ) ) ;
#7893 = ORIENTED_EDGE ( 'NONE', *, *, #7630, .T. ) ;
#7894 = CARTESIAN_POINT ( 'NONE',  ( -78.59375000204839523, 36.74823131438026280, 18.25176868561974786 ) ) ;
#7895 = CARTESIAN_POINT ( 'NONE',  ( 11.81093755974026394, 42.10901286868706705, 16.77394813616862734 ) ) ;
#7896 = ADVANCED_FACE ( 'NONE', ( #2178 ), #10324, .T. ) ;
#7897 = DIRECTION ( 'NONE',  ( 1.000000000000000000, -0.000000000000000000, 0.000000000000000000 ) ) ;
#7898 = EDGE_CURVE ( 'NONE', #1790, #8687, #11149, .T. ) ;
#7899 = CARTESIAN_POINT ( 'NONE',  ( 13.31285089744803862, 52.49279494320047235, 4.338208217070899764 ) ) ;
#7900 = CARTESIAN_POINT ( 'NONE',  ( -35.41758684555698267, 48.28175916350203067, -2.038952528722552504 ) ) ;
#7901 = EDGE_LOOP ( 'NONE', ( #11301, #9801, #9941 ) ) ;
#7902 = CARTESIAN_POINT ( 'NONE',  ( -45.81092964171354964, 71.80742102382775727, -12.92463648794852205 ) ) ;
#7903 = LINE ( 'NONE', #11593, #7776 ) ;
#7904 = FACE_OUTER_BOUND ( 'NONE', #2324, .T. ) ;
#7905 = EDGE_CURVE ( 'NONE', #11420, #8851, #9966, .T. ) ;
#7906 = CARTESIAN_POINT ( 'NONE',  ( -76.62500000204838102, 29.18810118750000626, -10.69163855873949132 ) ) ;
#7907 = DIRECTION ( 'NONE',  ( 1.000000000000000000, 0.000000000000000000, 0.000000000000000000 ) ) ;
#7908 = CARTESIAN_POINT ( 'NONE',  ( -72.40625000204839523, 36.74823131438026280, 18.25176868561974786 ) ) ;
#7909 = ORIENTED_EDGE ( 'NONE', *, *, #4193, .F. ) ;
#7910 = CARTESIAN_POINT ( 'NONE',  ( -75.78125000409680467, 65.35533905932737753, -24.99999999999999645 ) ) ;
#7911 = CARTESIAN_POINT ( 'NONE',  ( -80.00000000000001421, 50.75735931288069480, -5.742637315201482906 ) ) ;
#7912 = FACE_BOUND ( 'NONE', #479, .T. ) ;
#7913 = CARTESIAN_POINT ( 'NONE',  ( -30.11869220662914159, 34.20731585996448132, 3.085050890631813036 ) ) ;
#7914 = ORIENTED_EDGE ( 'NONE', *, *, #8165, .T. ) ;
#7915 = CARTESIAN_POINT ( 'NONE',  ( -77.75000000204839523, 80.81189881250000440, -10.69163855873948954 ) ) ;
#7916 = CARTESIAN_POINT ( 'NONE',  ( -20.00000000000003197, -63.00000000000000000, 5.000000000000000000 ) ) ;
#7917 = CARTESIAN_POINT ( 'NONE',  ( -15.00000000000000000, -30.00000000000000000, 10.00000000000000000 ) ) ;
#7918 = CARTESIAN_POINT ( 'NONE',  ( -30.36397657560652874, 35.99904827701746513, 8.986701095552454888 ) ) ;
#7919 = CARTESIAN_POINT ( 'NONE',  ( 4.180704885107411783, 3.359771601077107039, -5.901655677627842600 ) ) ;
#7920 = CARTESIAN_POINT ( 'NONE',  ( -77.28125000204838102, 55.00000000000000000, 25.81189881249999729 ) ) ;
#7921 = DIRECTION ( 'NONE',  ( -0.000000000000000000, -1.000000000000000000, -0.000000000000000000 ) ) ;
#7922 = ORIENTED_EDGE ( 'NONE', *, *, #1959, .F. ) ;
#7923 = CARTESIAN_POINT ( 'NONE',  ( 63.00000000000000000, 57.44550000000000267, 0.000000000000000000 ) ) ;
#7924 = ORIENTED_EDGE ( 'NONE', *, *, #10606, .T. ) ;
#7925 =( BOUNDED_CURVE ( )  B_SPLINE_CURVE ( 2, ( #1463, #7880, #7703, #8713, #5125, #552, #5907, #9550, #4218 ),
 .UNSPECIFIED., .F., .T. ) 
 B_SPLINE_CURVE_WITH_KNOTS ( ( 3, 2, 2, 2, 3 ),
 ( 0.3333333333333335924, 0.3541666666666669627, 0.3750000000000003331, 0.3958333333333336479, 0.4166666666666670182 ),
 .UNSPECIFIED. ) 
 CURVE ( )  GEOMETRIC_REPRESENTATION_ITEM ( )  RATIONAL_B_SPLINE_CURVE ( ( 0.9999999999999990008, 0.9238795325112877377, 1.000000000000000000, 0.9238795325112867385, 1.000000000000000000, 0.9238795325112867385, 1.000000000000000000, 0.9238795325112855172, 1.000000000000001110 ) ) 
 REPRESENTATION_ITEM ( '' )  );
#7926 = CARTESIAN_POINT ( 'NONE',  ( -58.04205566213050815, 55.34391004307462225, 6.992225127105330174 ) ) ;
#7927 = EDGE_CURVE ( 'NONE', #1664, #6455, #5609, .T. ) ;
#7928 = DIRECTION ( 'NONE',  ( 0.000000000000000000, -0.000000000000000000, 1.000000000000000000 ) ) ;
#7929 = CARTESIAN_POINT ( 'NONE',  ( -78.00000000000001421, 59.24264068711927678, 4.242644059037073312 ) ) ;
#7930 = PRODUCT_RELATED_PRODUCT_CATEGORY ( 'part', '', ( #3760 ) ) ;
#7931 = CARTESIAN_POINT ( 'NONE',  ( 13.89805254290603109, 70.85503171694512048, 15.26047230127977627 ) ) ;
#7932 = CARTESIAN_POINT ( 'NONE',  ( -74.56250000204839523, 80.81189881250000440, 10.69163855873948243 ) ) ;
#7933 = VERTEX_POINT ( 'NONE', #4703 ) ;
#7934 = CARTESIAN_POINT ( 'NONE',  ( -75.31250000204839523, 29.18810118750000981, 10.69163855873950020 ) ) ;
#7935 = ADVANCED_FACE ( 'NONE', ( #7472 ), #10203, .F. ) ;
#7936 = CARTESIAN_POINT ( 'NONE',  ( -77.75000000000000000, 55.00000000000000000, 24.99999999999999645 ) ) ;
#7937 = CARTESIAN_POINT ( 'NONE',  ( 52.99999999999999289, 55.00000000000000000, -2.999999999999999112 ) ) ;
#7938 = CARTESIAN_POINT ( 'NONE',  ( -19.49650547919373977, 55.00152523981414276, 0.004175815930542764627 ) ) ;
#7939 = CARTESIAN_POINT ( 'NONE',  ( -80.00000000000001421, 54.99999999999999289, -16.97055937655931501 ) ) ;
#7940 = ORIENTED_EDGE ( 'NONE', *, *, #4701, .T. ) ;
#7941 = CARTESIAN_POINT ( 'NONE',  ( -28.67970331391730454, 50.16047344865108215, 1.298006186689315999 ) ) ;
#7942 = CARTESIAN_POINT ( 'NONE',  ( -58.05785365788000263, 64.93276152744238061, 18.60033633024681521 ) ) ;
#7943 =( BOUNDED_CURVE ( )  B_SPLINE_CURVE ( 2, ( #1558, #5048, #5105, #419, #1387, #7741, #3297, #3125, #6852 ),
 .UNSPECIFIED., .F., .T. ) 
 B_SPLINE_CURVE_WITH_KNOTS ( ( 3, 2, 2, 2, 3 ),
 ( 0.6337432032608648624, 0.6535433226934000972, 0.6733434421259354430, 0.6931435615584705667, 0.7129436809910058015 ),
 .UNSPECIFIED. ) 
 CURVE ( )  GEOMETRIC_REPRESENTATION_ITEM ( )  RATIONAL_B_SPLINE_CURVE ( ( 1.000000000000000000, 0.9238795325112868495, 1.000000000000000000, 0.9238795325112868495, 1.000000000000000000, 0.9238795325112868495, 1.000000000000000000, 0.9238795325112868495, 1.000000000000000000 ) ) 
 REPRESENTATION_ITEM ( '' )  );
#7944 = ORIENTED_EDGE ( 'NONE', *, *, #4324, .F. ) ;
#7945 = CARTESIAN_POINT ( 'NONE',  ( -53.33716864159804771, 74.42687709403668350, 8.047385144602918317 ) ) ;
#7946 = CARTESIAN_POINT ( 'NONE',  ( -19.03633789442739399, 65.38143262936878841, 9.408964278925102676 ) ) ;
#7947 = CARTESIAN_POINT ( 'NONE',  ( -78.03125000204838102, 55.00000000000000000, -25.81189881249999729 ) ) ;
#7948 = VERTEX_POINT ( 'NONE', #6808 ) ;
#7949 = CARTESIAN_POINT ( 'NONE',  ( -72.21875000000001421, 80.00000000000001421, -10.35533905932737753 ) ) ;
#7950 = CARTESIAN_POINT ( 'NONE',  ( 5.451907626115248817, 34.19820075889870026, -3.085388827037094828 ) ) ;
#7951 = SHAPE_REPRESENTATION_RELATIONSHIP ( 'NONE' , 'NONE' ,  #6185, #7857 ) ;
#7952 = VERTEX_POINT ( 'NONE', #3198 ) ;
#7953 = DIRECTION ( 'NONE',  ( -1.000000000000000000, -6.033820786006286457E-17, -0.000000000000000000 ) ) ;
#7954 = CARTESIAN_POINT ( 'NONE',  ( 0.000000000000000000, 0.000000000000000000, -1.239675197676287643 ) ) ;
#7955 = CARTESIAN_POINT ( 'NONE',  ( -31.04203254678103718, 48.66984814105956758, 2.994375663034408053 ) ) ;
#7956 = ORIENTED_EDGE ( 'NONE', *, *, #1274, .F. ) ;
#7957 = CARTESIAN_POINT ( 'NONE',  ( 2.160190592651388908, 37.44772466133663613, -11.71846848753918913 ) ) ;
#7958 = DIRECTION ( 'NONE',  ( -1.000000000000000000, -0.000000000000000000, -0.000000000000000000 ) ) ;
#7959 = CARTESIAN_POINT ( 'NONE',  ( -80.00000000000000000, 55.00000000000000000, 0.000000000000000000 ) ) ;
#7960 = CARTESIAN_POINT ( 'NONE',  ( 0.000000000000000000, 50.00000000000000000, 0.000000000000000000 ) ) ;
#7961 = CARTESIAN_POINT ( 'NONE',  ( -71.84375000204838102, 55.00000000000000000, -25.81189881249999729 ) ) ;
#7962 = VERTEX_POINT ( 'NONE', #3372 ) ;
#7963 = CARTESIAN_POINT ( 'NONE',  ( -73.06250000409677625, 37.32233047033631124, -17.67766952966368166 ) ) ;
#7964 = DIRECTION ( 'NONE',  ( -1.000000000000000000, -0.000000000000000000, -0.000000000000000000 ) ) ;
#7965 = FACE_BOUND ( 'NONE', #4844, .T. ) ;
#7966 = CONICAL_SURFACE ( 'NONE', #2791, 5.000000000000000888, 1.047197551196596299 ) ;
#7967 = CARTESIAN_POINT ( 'NONE',  ( -3.608280849245335542, 57.05942974268126022, -21.01780866629736977 ) ) ;
#7968 = ORIENTED_EDGE ( 'NONE', *, *, #382, .F. ) ;
#7969 = CARTESIAN_POINT ( 'NONE',  ( -75.59375000204839523, 36.74823131438026280, 18.25176868561974786 ) ) ;
#7970 = AXIS2_PLACEMENT_3D ( 'NONE', #6977, #5058, #3134 ) ;
#7971 = CARTESIAN_POINT ( 'NONE',  ( -67.97817662023267360, 50.66675960002082491, 2.515712352184921841 ) ) ;
#7972 = CARTESIAN_POINT ( 'NONE',  ( 0.000000000000000000, 0.000000000000000000, -2.617914285714285416 ) ) ;
#7973 = CARTESIAN_POINT ( 'NONE',  ( -45.83980951013849392, 66.71822699054862937, -17.55167914569291554 ) ) ;
#7974 = DIRECTION ( 'NONE',  ( -1.000000000000000000, -0.000000000000000000, -0.000000000000000000 ) ) ;
#7975 = ADVANCED_FACE ( 'NONE', ( #10494 ), #4445, .T. ) ;
#7976 = CARTESIAN_POINT ( 'NONE',  ( -79.15625000204838102, 80.81189881250000440, -1.580522963032174394E-15 ) ) ;
#7977 = CARTESIAN_POINT ( 'NONE',  ( -78.00000000000000000, 54.99999999999999289, 1.500003371917797201 ) ) ;
#7978 = EDGE_LOOP ( 'NONE', ( #7821, #3536, #2146, #6824 ) ) ;
#7979 = AXIS2_PLACEMENT_3D ( 'NONE', #3003, #11009, #112 ) ;
#7980 = DIRECTION ( 'NONE',  ( 1.000000000000000000, 0.000000000000000000, 0.000000000000000000 ) ) ;
#7981 = EDGE_LOOP ( 'NONE', ( #6793, #4091, #11688, #4520, #11035, #8323 ) ) ;
#7982 = CARTESIAN_POINT ( 'NONE',  ( 25.33333333333333215, 69.00000000000001421, 0.000000000000000000 ) ) ;
#7983 = CARTESIAN_POINT ( 'NONE',  ( -77.18750000000007105, 37.32233047033638229, -17.67766952966361771 ) ) ;
#7984 = CARTESIAN_POINT ( 'NONE',  ( 2.500000000000003109, -4.330127018922193649, -6.099999999999999645 ) ) ;
#7985 = CARTESIAN_POINT ( 'NONE',  ( 5.696514063848578502, 66.13915503709409904, 18.97435054747177574 ) ) ;
#7986 = CARTESIAN_POINT ( 'NONE',  ( -71.53052369147287948, 77.35376373433385311, 12.90594309674112772 ) ) ;
#7987 = EDGE_LOOP ( 'NONE', ( #11194, #8734, #10621, #10763 ) ) ;
#7988 = CARTESIAN_POINT ( 'NONE',  ( -74.56250000204839523, 80.81189881250001861, -10.69163855873949132 ) ) ;
#7989 = EDGE_CURVE ( 'NONE', #10082, #9652, #8774, .T. ) ;
#7990 =( BOUNDED_CURVE ( )  B_SPLINE_CURVE ( 2, ( #5103, #1438, #8692, #474, #8749, #7855, #937, #2632, #10882 ),
 .UNSPECIFIED., .F., .T. ) 
 B_SPLINE_CURVE_WITH_KNOTS ( ( 3, 2, 2, 2, 3 ),
 ( 0.4753074076738947884, 0.4951072852372784272, 0.5149071628006619550, 0.5347070403640455938, 0.5545069179274292326 ),
 .UNSPECIFIED. ) 
 CURVE ( )  GEOMETRIC_REPRESENTATION_ITEM ( )  RATIONAL_B_SPLINE_CURVE ( ( 1.000000000000002220, 0.9238795325112845180, 1.000000000000000000, 0.9238795325112867385, 1.000000000000000000, 0.9238795325112867385, 1.000000000000000000, 0.9238795325113021706, 0.9999999999999845679 ) ) 
 REPRESENTATION_ITEM ( '' )  );
#7991 = CARTESIAN_POINT ( 'NONE',  ( 39.99999999999999289, 55.00000000000000000, 24.99999999999999645 ) ) ;
#7992 = CYLINDRICAL_SURFACE ( 'NONE', #10734, 1.499999999999999556 ) ;
#7993 = CARTESIAN_POINT ( 'NONE',  ( -5.795201733763983398, 54.99589100033183087, 0.003790395536194273666 ) ) ;
#7994 = AXIS2_PLACEMENT_3D ( 'NONE', #7157, #721, #6200 ) ;
#7995 =( NAMED_UNIT ( * ) PLANE_ANGLE_UNIT ( ) SI_UNIT ( $, .RADIAN. ) );
#7996 = COLOUR_RGB ( '',0.8941176470588234615, 0.8941176470588234615, 0.8941176470588234615 ) ;
#7997 = CARTESIAN_POINT ( 'NONE',  ( -75.00000000000002842, 29.64870206142003539, -2.722520311965037632 ) ) ;
#7998 = ORIENTED_EDGE ( 'NONE', *, *, #11517, .T. ) ;
#7999 = CARTESIAN_POINT ( 'NONE',  ( -75.12500000409677625, 55.00000000000000000, 24.99999999999999645 ) ) ;
#8000 = EDGE_CURVE ( 'NONE', #3514, #11523, #6088, .T. ) ;
#8001 = CARTESIAN_POINT ( 'NONE',  ( -80.00000000000001421, 67.72792206135787296, -12.72791868944004534 ) ) ;
#8002 = ORIENTED_EDGE ( 'NONE', *, *, #10682, .F. ) ;
#8003 = CARTESIAN_POINT ( 'NONE',  ( -30.88142570102377604, 34.60150157552137529, 5.109735466913361890 ) ) ;
#8004 = CARTESIAN_POINT ( 'NONE',  ( -54.33518187990853221, 67.95171888931189130, 5.365178638975860004 ) ) ;
#8005 = CARTESIAN_POINT ( 'NONE',  ( -76.53125000204838102, 55.00000000000000000, -25.81189881249999729 ) ) ;
#8006 = VECTOR ( 'NONE', #6613, 1000.000000000000000 ) ;
#8007 = VERTEX_POINT ( 'NONE', #11570 ) ;
#8008 = EDGE_CURVE ( 'NONE', #8906, #2384, #7693, .T. ) ;
#8009 = CARTESIAN_POINT ( 'NONE',  ( -77.93750000204838102, 65.69163855873948421, -25.81189881250000440 ) ) ;
#8010 = CARTESIAN_POINT ( 'NONE',  ( 47.00000000000000000, 105.0000000000000142, -6.000000000000000000 ) ) ;
#8011 = DIRECTION ( 'NONE',  ( 0.000000000000000000, 0.000000000000000000, 1.000000000000000000 ) ) ;
#8012 = DIRECTION ( 'NONE',  ( 0.000000000000000000, 0.000000000000000000, 1.000000000000000000 ) ) ;
#8013 = CARTESIAN_POINT ( 'NONE',  ( -79.90625000000001421, 65.35533905932736332, -24.99999999999996803 ) ) ;
#8014 = CARTESIAN_POINT ( 'NONE',  ( 6.426141312414339168, 55.01574567783170977, -0.004739632326276670311 ) ) ;
#8015 = ORIENTED_EDGE ( 'NONE', *, *, #6324, .T. ) ;
#8016 = CARTESIAN_POINT ( 'NONE',  ( -10.05849041713385716, 73.59815716747449699, -9.932440597164658769 ) ) ;
#8017 = DIRECTION ( 'NONE',  ( 0.000000000000000000, -0.000000000000000000, -1.000000000000000000 ) ) ;
#8018 = DIRECTION ( 'NONE',  ( 1.000000000000000000, 0.000000000000000000, 0.000000000000000000 ) ) ;
#8019 =( GEOMETRIC_REPRESENTATION_CONTEXT ( 3 ) GLOBAL_UNCERTAINTY_ASSIGNED_CONTEXT ( ( #8381 ) ) GLOBAL_UNIT_ASSIGNED_CONTEXT ( ( #3391, #1422, #3275 ) ) REPRESENTATION_CONTEXT ( 'NONE', 'WORKASPACE' ) );
#8020 = FACE_OUTER_BOUND ( 'NONE', #9031, .T. ) ;
#8021 = CARTESIAN_POINT ( 'NONE',  ( -74.18750000204839523, 65.69163855873949842, 25.81189881250000440 ) ) ;
#8022 = ORIENTED_EDGE ( 'NONE', *, *, #10655, .F. ) ;
#8023 = CARTESIAN_POINT ( 'NONE',  ( -74.84375000409679046, 30.00000000000001421, 10.35533905932739174 ) ) ;
#8024 = CARTESIAN_POINT ( 'NONE',  ( 53.00000000000000000, 51.46446609406726935, -3.535533905932738197 ) ) ;
#8025 = CARTESIAN_POINT ( 'NONE',  ( -78.00000000000001421, 50.75735931288069480, -5.742637315201482906 ) ) ;
#8026 = CARTESIAN_POINT ( 'NONE',  ( -57.82750524721426189, 59.10997802641301035, 20.69196764327204008 ) ) ;
#8027 = VECTOR ( 'NONE', #4302, 1000.000000000000000 ) ;
#8028 = EDGE_LOOP ( 'NONE', ( #11027, #8152, #10297, #4069 ) ) ;
#8029 = CARTESIAN_POINT ( 'NONE',  ( -75.96875000204839523, 73.25176868561975141, 18.25176868561974075 ) ) ;
#8030 = AXIS2_PLACEMENT_3D ( 'NONE', #2134, #8491, #1416 ) ;
#8031 = CARTESIAN_POINT ( 'NONE',  ( 19.99999999999996803, -63.00000000000000000, -5.000000000000000000 ) ) ;
#8032 = CARTESIAN_POINT ( 'NONE',  ( -2.500000000000000000, 3.061616997868383141E-16, -2.267810516609437776 ) ) ;
#8033 = CARTESIAN_POINT ( 'NONE',  ( 0.000000000000000000, 0.000000000000000000, -6.099999999999999645 ) ) ;
#8034 = AXIS2_PLACEMENT_3D ( 'NONE', #3935, #6708, #6823 ) ;
#8035 = CARTESIAN_POINT ( 'NONE',  ( -74.75000000204839523, 80.81189881250001861, -10.69163855873949132 ) ) ;
#8036 = CARTESIAN_POINT ( 'NONE',  ( 0.000000000000000000, 0.000000000000000000, 0.000000000000000000 ) ) ;
#8037 = CIRCLE ( 'NONE', #2864, 5.048155585660824229 ) ;
#8038 = VERTEX_POINT ( 'NONE', #11333 ) ;
#8039 = CARTESIAN_POINT ( 'NONE',  ( -78.00000000000001421, 54.99999999999998579, -8.485278002320759683 ) ) ;
#8040 = VERTEX_POINT ( 'NONE', #1403 ) ;
#8041 = CARTESIAN_POINT ( 'NONE',  ( 4.378415270005670656, 50.50465253094520790, -2.213690094899597227 ) ) ;
#8042 = CARTESIAN_POINT ( 'NONE',  ( -22.87290721160892559, 51.34344131888308738, 13.61233213364711858 ) ) ;
#8043 = CARTESIAN_POINT ( 'NONE',  ( -80.00000000000000000, 55.00000000000000000, -22.00000000000000000 ) ) ;
#8044 = FACE_OUTER_BOUND ( 'NONE', #2998, .T. ) ;
#8045 = DIRECTION ( 'NONE',  ( -1.000000000000000000, -0.000000000000000000, -0.000000000000000000 ) ) ;
#8046 = CARTESIAN_POINT ( 'NONE',  ( -75.03125000204838102, 55.00000000000000000, -25.81189881249999729 ) ) ;
#8047 = ORIENTED_EDGE ( 'NONE', *, *, #2613, .T. ) ;
#8048 = PRESENTATION_STYLE_ASSIGNMENT (( #4397 ) ) ;
#8049 = CARTESIAN_POINT ( 'NONE',  ( -76.71875000204839523, 29.18810118750000271, 4.741568889096522788E-15 ) ) ;
#8050 = EDGE_CURVE ( 'NONE', #3861, #1195, #496, .T. ) ;
#8051 = DIRECTION ( 'NONE',  ( -1.000000000000000000, -0.000000000000000000, -0.000000000000000000 ) ) ;
#8052 = AXIS2_PLACEMENT_3D ( 'NONE', #10210, #3927, #3873 ) ;
#8053 = CARTESIAN_POINT ( 'NONE',  ( -76.90625000409677625, 80.00000000000001421, 10.35533905932737397 ) ) ;
#8054 = CARTESIAN_POINT ( 'NONE',  ( -10.57393008609709284, 54.97382464119526446, -0.001646660502260763022 ) ) ;
#8055 = DIRECTION ( 'NONE',  ( 0.000000000000000000, 0.000000000000000000, 1.000000000000000000 ) ) ;
#8056 = CARTESIAN_POINT ( 'NONE',  ( -78.00000000000001421, 63.48528137423857487, -6.985278002320760571 ) ) ;
#8057 = CIRCLE ( 'NONE', #7874, 3.000000000000000000 ) ;
#8058 = ORIENTED_EDGE ( 'NONE', *, *, #5067, .F. ) ;
#8059 = CARTESIAN_POINT ( 'NONE',  ( -16.62112305147868341, 58.30599534545817875, 3.765284532852771537 ) ) ;
#8060 = AXIS2_PLACEMENT_3D ( 'NONE', #9890, #11625, #4274 ) ;
#8061 = CARTESIAN_POINT ( 'NONE',  ( 2.925285743277525885, 4.084588180558403003, -0.01055556052338900083 ) ) ;
#8062 = EDGE_LOOP ( 'NONE', ( #10972, #11022 ) ) ;
#8063 = CARTESIAN_POINT ( 'NONE',  ( -58.60805698665915742, 61.13948054013681599, 20.20364628154455033 ) ) ;
#8064 = CARTESIAN_POINT ( 'NONE',  ( -75.96875000204839523, 73.25176868561975141, 18.25176868561974075 ) ) ;
#8065 = EDGE_CURVE ( 'NONE', #3965, #7948, #8659, .T. ) ;
#8066 = EDGE_CURVE ( 'NONE', #89, #2849, #5400, .T. ) ;
#8067 = ADVANCED_FACE ( 'NONE', ( #616, #5243 ), #9665, .T. ) ;
#8068 = AXIS2_PLACEMENT_3D ( 'NONE', #2964, #1277, #8602 ) ;
#8069 = CIRCLE ( 'NONE', #9390, 5.000000000000000888 ) ;
#8070 = ORIENTED_EDGE ( 'NONE', *, *, #10002, .F. ) ;
#8071 = PRODUCT_DEFINITION_SHAPE ( 'NONE', 'NONE',  #2197 ) ;
#8072 = CARTESIAN_POINT ( 'NONE',  ( -71.75000000204838102, 80.81189881250001861, -10.69163855873949132 ) ) ;
#8073 = CARTESIAN_POINT ( 'NONE',  ( 19.52230480204648799, 67.92440004991483704, 16.80766691833610693 ) ) ;
#8074 = EDGE_CURVE ( 'NONE', #1664, #8222, #1517, .T. ) ;
#8075 = EDGE_CURVE ( 'NONE', #11030, #541, #5204, .T. ) ;
#8076 = CARTESIAN_POINT ( 'NONE',  ( 0.000000000000000000, 0.000000000000000000, -6.074599999999999334 ) ) ;
#8077 = CARTESIAN_POINT ( 'NONE',  ( 12.53471759186635914, 51.95107372724174155, 3.976201241736514902 ) ) ;
#8078 = AXIS2_PLACEMENT_3D ( 'NONE', #6986, #11629, #6325 ) ;
#8079 = CARTESIAN_POINT ( 'NONE',  ( -63.41718291383947559, 52.96799456708508558, 6.699226218324908722 ) ) ;
#8080 = VERTEX_POINT ( 'NONE', #2481 ) ;
#8081 = ADVANCED_FACE ( 'NONE', ( #4155 ), #7312, .T. ) ;
#8082 = CARTESIAN_POINT ( 'NONE',  ( -60.45014771802851072, 49.89223742090062075, 20.38901927491476584 ) ) ;
#8083 = CARTESIAN_POINT ( 'NONE',  ( -20.45202553191040806, 65.80759480864719535, 18.03021102644938267 ) ) ;
#8084 = CARTESIAN_POINT ( 'NONE',  ( 0.000000000000000000, 50.00000000000000000, 20.00000000000000000 ) ) ;
#8085 = DIRECTION ( 'NONE',  ( -1.000000000000000000, -0.000000000000000000, -0.000000000000000000 ) ) ;
#8086 = DIRECTION ( 'NONE',  ( -0.000000000000000000, 0.000000000000000000, -1.000000000000000000 ) ) ;
#8087 = B_SPLINE_CURVE_WITH_KNOTS ( 'NONE', 3,
 ( #11316, #1386, #1439, #1499 ),
 .UNSPECIFIED., .F., .F.,
 ( 4, 4 ),
 ( 2.380735201026667963E-07, 0.002921158011986725936 ),
 .UNSPECIFIED. ) ;
#8088 = ORIENTED_EDGE ( 'NONE', *, *, #8943, .F. ) ;
#8089 = DIRECTION ( 'NONE',  ( 0.000000000000000000, 0.000000000000000000, 1.000000000000000000 ) ) ;
#8090 = FACE_BOUND ( 'NONE', #8539, .T. ) ;
#8091 = CARTESIAN_POINT ( 'NONE',  ( -39.16026728571524984, 50.89059911655681390, -20.69167526169209026 ) ) ;
#8092 = ORIENTED_EDGE ( 'NONE', *, *, #190, .F. ) ;
#8093 = CARTESIAN_POINT ( 'NONE',  ( -80.00000000000000000, 55.00000000000000000, 0.000000000000000000 ) ) ;
#8094 = PLANE ( 'NONE',  #10061 ) ;
#8095 = ORIENTED_EDGE ( 'NONE', *, *, #2500, .T. ) ;
#8096 = CARTESIAN_POINT ( 'NONE',  ( 0.000000000000000000, 0.000000000000000000, -5.560532340533429263 ) ) ;
#8097 = CARTESIAN_POINT ( 'NONE',  ( 52.99999999999999289, 97.00000000000000000, -9.797174393178809880E-16 ) ) ;
#8098 = CARTESIAN_POINT ( 'NONE',  ( -76.43750000204838102, 65.69163855873948421, -25.81189881250000440 ) ) ;
#8099 = CARTESIAN_POINT ( 'NONE',  ( -76.15625000204838102, 80.81189881250000440, -1.580522963032174394E-15 ) ) ;
#8100 = ORIENTED_EDGE ( 'NONE', *, *, #5718, .T. ) ;
#8101 = DIRECTION ( 'NONE',  ( 1.000000000000000000, 0.000000000000000000, 0.000000000000000000 ) ) ;
#8102 = ORIENTED_EDGE ( 'NONE', *, *, #6324, .F. ) ;
#8103 = CARTESIAN_POINT ( 'NONE',  ( 2.818321079511319827, 51.23034582308294915, -3.301094900672958410 ) ) ;
#8104 = CARTESIAN_POINT ( 'NONE',  ( -1.872832575621271589, 53.16883357371531105, -13.97545723436864762 ) ) ;
#8105 = DIRECTION ( 'NONE',  ( 0.000000000000000000, 0.000000000000000000, -1.000000000000000000 ) ) ;
#8106 = DIRECTION ( 'NONE',  ( 0.000000000000000000, 1.000000000000000000, 0.000000000000000000 ) ) ;
#8107 = CARTESIAN_POINT ( 'NONE',  ( -78.00000000000001421, 63.48528137423857487, -1.499996628082204797 ) ) ;
#8108 = CARTESIAN_POINT ( 'NONE',  ( -74.46875000204839523, 73.25176868561975141, 18.25176868561974075 ) ) ;
#8109 = VERTEX_POINT ( 'NONE', #6030 ) ;
#8110 = CARTESIAN_POINT ( 'NONE',  ( -76.06250000409679046, 37.32233047033631124, -17.67766952966368166 ) ) ;
#8111 = CARTESIAN_POINT ( 'NONE',  ( -76.43750000204839523, 44.30836144126050158, -25.81189881249999374 ) ) ;
#8112 = EDGE_CURVE ( 'NONE', #884, #9742, #7925, .T. ) ;
#8113 = CARTESIAN_POINT ( 'NONE',  ( 52.99999999999999289, 58.53553390593273065, 3.535533905932731091 ) ) ;
#8114 = CARTESIAN_POINT ( 'NONE',  ( -30.28557338859272718, 54.99143721797869944, -0.0008624110448812779411 ) ) ;
#8115 = CARTESIAN_POINT ( 'NONE',  ( -9.472297265023270185, 67.98144036619800090, -17.76723545671738336 ) ) ;
#8116 = EDGE_LOOP ( 'NONE', ( #5033, #7877, #1257, #6465 ) ) ;
#8117 = DIRECTION ( 'NONE',  ( 0.000000000000000000, 1.000000000000000000, 0.000000000000000000 ) ) ;
#8118 = VECTOR ( 'NONE', #638, 1000.000000000000000 ) ;
#8119 = DIRECTION ( 'NONE',  ( 0.000000000000000000, 1.000000000000000000, 0.000000000000000000 ) ) ;
#8120 = ORIENTED_EDGE ( 'NONE', *, *, #602, .F. ) ;
#8121 = CARTESIAN_POINT ( 'NONE',  ( -59.16083848046626059, 59.10996271935812274, 20.69255083878625712 ) ) ;
#8122 = CARTESIAN_POINT ( 'NONE',  ( -74.75000000204839523, 80.81189881250001861, -10.69163855873949132 ) ) ;
#8123 = ORIENTED_EDGE ( 'NONE', *, *, #4702, .F. ) ;
#8124 = CARTESIAN_POINT ( 'NONE',  ( -71.93750000204838102, 65.69163855873948421, -25.81189881250000440 ) ) ;
#8125 = CARTESIAN_POINT ( 'NONE',  ( -13.14429486149114013, 76.02373996650987920, 2.745652855075435994 ) ) ;
#8126 = ORIENTED_EDGE ( 'NONE', *, *, #3062, .F. ) ;
#8127 = CYLINDRICAL_SURFACE ( 'NONE', #5527, 1.500000000000000000 ) ;
#8128 = CARTESIAN_POINT ( 'NONE',  ( 16.57387832582033838, 55.01040436726604810, 0.01274895920632791203 ) ) ;
#8129 = ORIENTED_EDGE ( 'NONE', *, *, #8476, .T. ) ;
#8130 = CARTESIAN_POINT ( 'NONE',  ( -4.826933883979098283, 59.12189523993642126, -20.68950996840993284 ) ) ;
#8131 = CARTESIAN_POINT ( 'NONE',  ( -9.070746587277097817, 68.33487957594263662, -16.24597445391072270 ) ) ;
#8132 = DIRECTION ( 'NONE',  ( 1.000000000000000000, 0.000000000000000000, 0.000000000000000000 ) ) ;
#8133 = CARTESIAN_POINT ( 'NONE',  ( -80.00000000000000000, 55.00000000000000000, 0.000000000000000000 ) ) ;
#8134 = CARTESIAN_POINT ( 'NONE',  ( -4.592054218142292754, -3.122278952918454920, -5.789399939901068493 ) ) ;
#8135 = EDGE_CURVE ( 'NONE', #849, #3307, #1345, .T. ) ;
#8136 = ORIENTED_EDGE ( 'NONE', *, *, #587, .T. ) ;
#8137 = CARTESIAN_POINT ( 'NONE',  ( -78.00000000000001421, 59.24264068711927678, -2.742637315201482462 ) ) ;
#8138 = DIRECTION ( 'NONE',  ( 0.000000000000000000, -1.000000000000000000, 0.000000000000000000 ) ) ;
#8139 = MECHANICAL_DESIGN_GEOMETRIC_PRESENTATION_REPRESENTATION (  '', ( #1440 ), #3544 ) ;
#8140=STYLED_ITEM('',(#11874),#980);
#8141 = ORIENTED_EDGE ( 'NONE', *, *, #7567, .F. ) ;
#8142 = DIRECTION ( 'NONE',  ( 1.000000000000000000, 6.033820786006286457E-17, 0.000000000000000000 ) ) ;
#8143 = CARTESIAN_POINT ( 'NONE',  ( -62.53961969342599048, 54.34518536178778447, 4.967644874103720909 ) ) ;
#8144 = ADVANCED_FACE ( 'NONE', ( #5975 ), #11113, .F. ) ;
#8145 = EDGE_LOOP ( 'NONE', ( #8916, #5724, #1587, #1040 ) ) ;
#8146 = CARTESIAN_POINT ( 'NONE',  ( 36.99999999999999289, 50.00000000000001421, 6.123233995736750505E-16 ) ) ;
#8147 = CARTESIAN_POINT ( 'NONE',  ( 0.000000000000000000, 0.000000000000000000, -6.099999999999999645 ) ) ;
#8148 = CARTESIAN_POINT ( 'NONE',  ( 21.45655948015391701, 59.96735746368497644, 0.6566347522681182936 ) ) ;
#8149 = CARTESIAN_POINT ( 'NONE',  ( -78.40625000204838102, 29.18810118750000271, 4.741568889096522788E-15 ) ) ;
#8150 = CARTESIAN_POINT ( 'NONE',  ( -79.34375000204839523, 73.25176868561975141, -18.25176868561974430 ) ) ;
#8151 = CIRCLE ( 'NONE', #5101, 3.000000000000000000 ) ;
#8152 = ORIENTED_EDGE ( 'NONE', *, *, #8074, .T. ) ;
#8153 = CARTESIAN_POINT ( 'NONE',  ( -79.34375000204839523, 55.00000000000000000, -25.81189881249999729 ) ) ;
#8154 = VERTEX_POINT ( 'NONE', #10732 ) ;
#8155 = CARTESIAN_POINT ( 'NONE',  ( 19.48027454407776915, 75.17671222592493052, 14.77705221063085617 ) ) ;
#8156 = CARTESIAN_POINT ( 'NONE',  ( 2.595294705192281892, 44.14252394839951421, -8.915488700345314044 ) ) ;
#8157 = CARTESIAN_POINT ( 'NONE',  ( -75.78125000204839523, 73.25176868561975141, 18.25176868561974075 ) ) ;
#8158 = CARTESIAN_POINT ( 'NONE',  ( -77.18750000409679046, 72.67766952966368876, -17.67766952966368876 ) ) ;
#8159 = CIRCLE ( 'NONE', #9684, 4.999999999999995559 ) ;
#8160 = DIRECTION ( 'NONE',  ( -1.000000000000000000, -0.000000000000000000, -0.000000000000000000 ) ) ;
#8161 = ORIENTED_EDGE ( 'NONE', *, *, #996, .T. ) ;
#8162 = AXIS2_PLACEMENT_3D ( 'NONE', #369, #2406, #9773 ) ;
#8163 = SURFACE_STYLE_USAGE ( .BOTH. , #2716 ) ;
#8164 = CARTESIAN_POINT ( 'NONE',  ( -75.40625000409677625, 80.00000000000001421, 10.35533905932737397 ) ) ;
#8165 = EDGE_CURVE ( 'NONE', #10833, #1407, #9136, .T. ) ;
#8166 = CARTESIAN_POINT ( 'NONE',  ( -15.09523335307150838, 60.00000000000000000, 4.640896189903090912E-12 ) ) ;
#8167 = CARTESIAN_POINT ( 'NONE',  ( -80.00000000000000000, 55.00000000000000000, 0.000000000000000000 ) ) ;
#8168 = CARTESIAN_POINT ( 'NONE',  ( -56.83651104956651778, 55.00013208380096330, -0.005320426939399679200 ) ) ;
#8169 = ITEM_DEFINED_TRANSFORMATION ( 'NONE', 'NONE', #4883,  #4738 ) ;
#8170 = CARTESIAN_POINT ( 'NONE',  ( -0.7352373834349590354, 64.99605696851786263, -19.59792961213366169 ) ) ;
#8171 = AXIS2_PLACEMENT_3D ( 'NONE', #7271, #10722, #8106 ) ;
#8172 = CARTESIAN_POINT ( 'NONE',  ( -19.34581284733777551, 56.29866528490898503, 4.839339984244626081 ) ) ;
#8173 = AXIS2_PLACEMENT_3D ( 'NONE', #11240, #1244, #3950 ) ;
#8174 = EDGE_LOOP ( 'NONE', ( #2074, #6606, #4562, #2278 ) ) ;
#8175 = CARTESIAN_POINT ( 'NONE',  ( 9.999999999999994671, -30.00000000000000000, 10.00000000000000000 ) ) ;
#8176 = VERTEX_POINT ( 'NONE', #9898 ) ;
#8177 = CARTESIAN_POINT ( 'NONE',  ( 16.81101720596863203, 65.56606704192360269, 18.33326034385300574 ) ) ;
#8178 = CARTESIAN_POINT ( 'NONE',  ( -72.21875000204838102, 36.74823131438024859, -18.25176868561973720 ) ) ;
#8179 = CIRCLE ( 'NONE', #2630, 1.500000000000001332 ) ;
#8180 = CIRCLE ( 'NONE', #10653, 5.000000000000000000 ) ;
#8181 = ORIENTED_EDGE ( 'NONE', *, *, #1316, .F. ) ;
#8182 = EDGE_CURVE ( 'NONE', #6801, #6451, #8259, .T. ) ;
#8183 = CARTESIAN_POINT ( 'NONE',  ( -74.37500000204838102, 65.69163855873949842, 25.81189881250000440 ) ) ;
#8184 = CARTESIAN_POINT ( 'NONE',  ( -3.608280849245335542, 57.05942974268126022, -21.01780866629736977 ) ) ;
#8185 = ORIENTED_EDGE ( 'NONE', *, *, #9896, .F. ) ;
#8186 = DIRECTION ( 'NONE',  ( 1.000000000000000000, 6.033820786006286457E-17, 0.000000000000000000 ) ) ;
#8187 = CARTESIAN_POINT ( 'NONE',  ( 5.097072204971999199, 54.98817743756426779, 0.003549163818565345425 ) ) ;
#8188 = AXIS2_PLACEMENT_3D ( 'NONE', #765, #651, #11784 ) ;
#8189 = EDGE_LOOP ( 'NONE', ( #4954, #6222 ) ) ;
#8190 = CARTESIAN_POINT ( 'NONE',  ( -66.81799029952708224, 34.52069382205590387, 5.503409927558503334 ) ) ;
#8191 = CARTESIAN_POINT ( 'NONE',  ( -27.52231952827322559, 42.10572610250680015, 16.77759997522909785 ) ) ;
#8192 = CARTESIAN_POINT ( 'NONE',  ( 5.000000000000000000, 2.886751345948134428, -5.653418012614792154 ) ) ;
#8193 = SURFACE_SIDE_STYLE ('',( #6523 ) ) ;
#8194 = LINE ( 'NONE', #7249, #2862 ) ;
#8195 = CARTESIAN_POINT ( 'NONE',  ( -3.556264818047240706, -3.720292241887095397, -6.018341802876227220 ) ) ;
#8196 = EDGE_CURVE ( 'NONE', #2740, #1955, #9605, .T. ) ;
#8197 = VERTEX_POINT ( 'NONE', #4461 ) ;
#8198 = CARTESIAN_POINT ( 'NONE',  ( -71.00000000409677625, 80.00000000000000000, -1.530808498934191324E-15 ) ) ;
#8199 = CARTESIAN_POINT ( 'NONE',  ( -51.09272475326343965, 55.01575874039146896, -0.004732945744491365812 ) ) ;
#8200 = CARTESIAN_POINT ( 'NONE',  ( -46.38003273829423279, 59.55718620543969877, -2.063744646361077795 ) ) ;
#8201 = FACE_OUTER_BOUND ( 'NONE', #2029, .T. ) ;
#8202 = CARTESIAN_POINT ( 'NONE',  ( -57.48338928910774825, 58.30336033756839953, 3.767575935608591386 ) ) ;
#8203 = ORIENTED_EDGE ( 'NONE', *, *, #2947, .T. ) ;
#8204 = DIRECTION ( 'NONE',  ( 1.000000000000000000, 6.033820786006286457E-17, -0.000000000000000000 ) ) ;
#8205 = FACE_OUTER_BOUND ( 'NONE', #11078, .T. ) ;
#8206 = CARTESIAN_POINT ( 'NONE',  ( 14.84754529999163175, 56.60743895240869961, 4.745939591966136462 ) ) ;
#8207 = CARTESIAN_POINT ( 'NONE',  ( -71.65625000204838102, 80.81189881250000440, -1.580522963032174394E-15 ) ) ;
#8208 = CARTESIAN_POINT ( 'NONE',  ( -76.90625000204838102, 29.18810118750000271, 4.741568889096522788E-15 ) ) ;
#8209 = ADVANCED_FACE ( 'NONE', ( #11071 ), #1694, .F. ) ;
#8210 = ORIENTED_EDGE ( 'NONE', *, *, #9645, .F. ) ;
#8211 = EDGE_CURVE ( 'NONE', #7233, #9521, #2540, .T. ) ;
#8212 = CARTESIAN_POINT ( 'NONE',  ( -74.75000000204840944, 65.69163855873948421, -25.81189881250000440 ) ) ;
#8213 = EDGE_LOOP ( 'NONE', ( #1458, #1433, #6812, #9504 ) ) ;
#8214 = CARTESIAN_POINT ( 'NONE',  ( -7.676230545052211696, 58.97267896026763623, -3.053804416834208890 ) ) ;
#8215 = CIRCLE ( 'NONE', #6881, 1.500000000000001332 ) ;
#8216 = CARTESIAN_POINT ( 'NONE',  ( -18.41060825077335394, 61.60246496029746766, 12.35359534585878549 ) ) ;
#8217 = CARTESIAN_POINT ( 'NONE',  ( -77.00000000204839523, 44.30836144126052289, 25.81189881250000795 ) ) ;
#8218 = CARTESIAN_POINT ( 'NONE',  ( -76.90625000409677625, 80.00000000000001421, 10.35533905932737397 ) ) ;
#8219 = DIRECTION ( 'NONE',  ( -0.04756514941544910668, -0.9988681377244376103, 0.000000000000000000 ) ) ;
#8220 = CIRCLE ( 'NONE', #9357, 29.00000000000000355 ) ;
#8221 = AXIS2_PLACEMENT_3D ( 'NONE', #5099, #8401, #5943 ) ;
#8222 = VERTEX_POINT ( 'NONE', #5416 ) ;
#8223 = ADVANCED_FACE ( 'NONE', ( #9009 ), #2337, .F. ) ;
#8224 = CARTESIAN_POINT ( 'NONE',  ( -71.53052369147287948, 77.35376373433385311, 12.90594309674112772 ) ) ;
#8225 = CARTESIAN_POINT ( 'NONE',  ( -78.21875000409679046, 65.35533905932737753, 24.99999999999999645 ) ) ;
#8226 = LINE ( 'NONE', #3611, #10928 ) ;
#8227 = CARTESIAN_POINT ( 'NONE',  ( -49.83687785813567928, 54.99470118834590693, -0.002487210696061862344 ) ) ;
#8228 = APPLICATION_PROTOCOL_DEFINITION ( 'draft international standard', 'automotive_design', 1998, #1636 ) ;
#8229 = AXIS2_PLACEMENT_3D ( 'NONE', #4263, #7921, #1503 ) ;
#8230 = CARTESIAN_POINT ( 'NONE',  ( -18.91777915131708454, 74.69377696386850118, -9.811015657242856847 ) ) ;
#8231 = CARTESIAN_POINT ( 'NONE',  ( -12.35069320478294230, 59.96772244320774092, 0.6536033618355622243 ) ) ;
#8232 = ORIENTED_EDGE ( 'NONE', *, *, #6915, .T. ) ;
#8233 = CARTESIAN_POINT ( 'NONE',  ( -78.00000000000001421, 42.27207793864211283, -14.22791868944003646 ) ) ;
#8234 = ORIENTED_EDGE ( 'NONE', *, *, #3378, .T. ) ;
#8235 = CARTESIAN_POINT ( 'NONE',  ( -17.82693376281896391, 72.53768310958322729, 11.72612467905221934 ) ) ;
#8236 = CIRCLE ( 'NONE', #5565, 2.500000000000000000 ) ;
#8237 = CARTESIAN_POINT ( 'NONE',  ( -78.59375000204839523, 55.00000000000000000, 25.81189881249999729 ) ) ;
#8238 = ORIENTED_EDGE ( 'NONE', *, *, #8684, .F. ) ;
#8239 = CARTESIAN_POINT ( 'NONE',  ( -75.40625000204838102, 29.18810118750000271, 4.741568889096522788E-15 ) ) ;
#8240 = CARTESIAN_POINT ( 'NONE',  ( -34.14426257084027583, 36.62727174719971401, -10.58198811264723282 ) ) ;
#8241 = AXIS2_PLACEMENT_3D ( 'NONE', #6322, #1751, #5415 ) ;
#8242 = ORIENTED_EDGE ( 'NONE', *, *, #11792, .T. ) ;
#8243 = AXIS2_PLACEMENT_3D ( 'NONE', #3833, #343, #9334 ) ;
#8244 = DIRECTION ( 'NONE',  ( -1.000000000000000000, -0.000000000000000000, -0.000000000000000000 ) ) ;
#8245 = CARTESIAN_POINT ( 'NONE',  ( -70.22791978040648075, 48.01650020567630150, 0.9109789678819780745 ) ) ;
#8246 = EDGE_LOOP ( 'NONE', ( #6667, #7323, #2676, #5787, #6060 ) ) ;
#8247 = CARTESIAN_POINT ( 'NONE',  ( -32.83980940775745694, 34.29934832242292231, -4.109488215307584014 ) ) ;
#8248 = AXIS2_PLACEMENT_3D ( 'NONE', #5886, #3961, #3063 ) ;
#8249 = CARTESIAN_POINT ( 'NONE',  ( -10.83980928483403794, 72.54296691076741865, -11.73126556815853760 ) ) ;
#8250 = FACE_OUTER_BOUND ( 'NONE', #6178, .T. ) ;
#8251 = FACE_OUTER_BOUND ( 'NONE', #11349, .T. ) ;
#8252 = DIRECTION ( 'NONE',  ( -1.000000000000000000, -0.000000000000000000, -0.000000000000000000 ) ) ;
#8253 = ORIENTED_EDGE ( 'NONE', *, *, #6601, .F. ) ;
#8254 = EDGE_CURVE ( 'NONE', #1114, #3047, #7224, .T. ) ;
#8255 = CARTESIAN_POINT ( 'NONE',  ( -71.28125000409676204, 65.35533905932761911, -24.99999999999974420 ) ) ;
#8256 = CARTESIAN_POINT ( 'NONE',  ( -45.95223880245733028, 55.00272212807455929, -0.004616914605015018727 ) ) ;
#8257 = CARTESIAN_POINT ( 'NONE',  ( -43.46451671436751241, 58.04975000076846925, -3.975644651036446486 ) ) ;
#8258 = AXIS2_PLACEMENT_3D ( 'NONE', #11780, #4603, #6409 ) ;
#8259 = CIRCLE ( 'NONE', #4624, 3.000000000000000000 ) ;
#8260 = DIRECTION ( 'NONE',  ( -0.000000000000000000, -0.000000000000000000, -1.000000000000000000 ) ) ;
#8261 = CARTESIAN_POINT ( 'NONE',  ( -80.00000000000002842, 50.75735931288069480, 12.72792543327563131 ) ) ;
#8262 = ORIENTED_EDGE ( 'NONE', *, *, #3103, .T. ) ;
#8263 = DIRECTION ( 'NONE',  ( 0.000000000000000000, 0.000000000000000000, 1.000000000000000000 ) ) ;
#8264 = CARTESIAN_POINT ( 'NONE',  ( -33.76207074264209496, 50.00000000000002842, -7.785926851161516095E-15 ) ) ;
#8265 = CARTESIAN_POINT ( 'NONE',  ( 11.34649352705233305, 53.70496425952375574, 4.840325120478907728 ) ) ;
#8266 = EDGE_CURVE ( 'NONE', #8197, #10439, #9784, .T. ) ;
#8267 = CARTESIAN_POINT ( 'NONE',  ( -3.411829342377862062, 65.82156647569453867, -22.53680681160409094 ) ) ;
#8268 = CARTESIAN_POINT ( 'NONE',  ( -77.00000000204838102, 29.18810118750000981, 10.69163855873950020 ) ) ;
#8269 = ORIENTED_EDGE ( 'NONE', *, *, #6263, .F. ) ;
#8270 = CARTESIAN_POINT ( 'NONE',  ( -77.18750000204839523, 65.69163855873949842, 25.81189881250000440 ) ) ;
#8271 = ORIENTED_EDGE ( 'NONE', *, *, #8368, .F. ) ;
#8272 = CARTESIAN_POINT ( 'NONE',  ( -1.847600398352776008, 54.66814614765320357, -4.991699084503711248 ) ) ;
#8273 = CARTESIAN_POINT ( 'NONE',  ( -16.66853507982470717, 64.91323907223390677, 9.913723736632611860 ) ) ;
#8274 = CARTESIAN_POINT ( 'NONE',  ( -76.71875000204839523, 29.18810118750000271, 4.741568889096522788E-15 ) ) ;
#8275 = LINE ( 'NONE', #11133, #11215 ) ;
#8276 = CARTESIAN_POINT ( 'NONE',  ( 2.500000000000000000, 0.000000000000000000, -1.239675197676287643 ) ) ;
#8277 = ORIENTED_EDGE ( 'NONE', *, *, #11026, .F. ) ;
#8278 = CARTESIAN_POINT ( 'NONE',  ( -79.34375000000002842, 65.35533905932737753, 24.99999999999999645 ) ) ;
#8279 = CARTESIAN_POINT ( 'NONE',  ( -71.65625000204839523, 73.25176868561975141, -18.25176868561974430 ) ) ;
#8280 = DIRECTION ( 'NONE',  ( 0.000000000000000000, 1.000000000000000000, 0.000000000000000000 ) ) ;
#8281 = EDGE_CURVE ( 'NONE', #443, #5990, #3278, .T. ) ;
#8282 = CARTESIAN_POINT ( 'NONE',  ( -47.90718171337187670, 54.97383743986804916, -0.001639851572109073119 ) ) ;
#8283 = APPLICATION_PROTOCOL_DEFINITION ( 'draft international standard', 'automotive_design', 1998, #5550 ) ;
#8284 = CARTESIAN_POINT ( 'NONE',  ( -8.864316419551519388, 67.63873506485967368, -18.01151076427558806 ) ) ;
#8285 = DIRECTION ( 'NONE',  ( 0.000000000000000000, 1.000000000000000000, 0.000000000000000000 ) ) ;
#8286 = VERTEX_POINT ( 'NONE', #2881 ) ;
#8287 = DIRECTION ( 'NONE',  ( -0.000000000000000000, -0.000000000000000000, -1.000000000000000000 ) ) ;
#8288 = ADVANCED_FACE ( 'NONE', ( #4342 ), #7992, .F. ) ;
#8289 = DIRECTION ( 'NONE',  ( 0.000000000000000000, 1.000000000000000000, 0.000000000000000000 ) ) ;
#8290 = EDGE_CURVE ( 'NONE', #11481, #2610, #5987, .T. ) ;
#8291 = EDGE_LOOP ( 'NONE', ( #4526, #7348, #8527, #9609 ) ) ;
#8292 = CARTESIAN_POINT ( 'NONE',  ( 0.2748429140369315071, 38.70467982241823535, -13.38321124372595783 ) ) ;
#8293 = CARTESIAN_POINT ( 'NONE',  ( -77.56250000204839523, 80.81189881250001861, -10.69163855873949132 ) ) ;
#8294 = ORIENTED_EDGE ( 'NONE', *, *, #10321, .T. ) ;
#8295 = CARTESIAN_POINT ( 'NONE',  ( -75.68750000204838102, 44.30836144126053000, 25.81189881250000795 ) ) ;
#8296 = CARTESIAN_POINT ( 'NONE',  ( -19.63602748969081446, 62.08618401115764129, 19.80343740535094099 ) ) ;
#8297 = DIRECTION ( 'NONE',  ( -0.000000000000000000, -0.000000000000000000, -1.000000000000000000 ) ) ;
#8298 = EDGE_LOOP ( 'NONE', ( #10077, #7462, #4518, #11738 ) ) ;
#8299 = AXIS2_PLACEMENT_3D ( 'NONE', #6649, #2077, #5751 ) ;
#8300 = CARTESIAN_POINT ( 'NONE',  ( -11.98451233991428744, 59.33800141420930885, -2.507694870718707225 ) ) ;
#8301 = CARTESIAN_POINT ( 'NONE',  ( 3.737309610555803463, 34.06887424008940712, -2.059134394038261817 ) ) ;
#8302 = ORIENTED_EDGE ( 'NONE', *, *, #8684, .T. ) ;
#8303 = CARTESIAN_POINT ( 'NONE',  ( -54.11877253047997982, 71.88441139826683468, 12.52138966593202341 ) ) ;
#8304 = CARTESIAN_POINT ( 'NONE',  ( -44.96936008568403764, 63.99178041037959019, -19.01235157881157178 ) ) ;
#8305 = DIRECTION ( 'NONE',  ( 0.000000000000000000, 0.9848077530122080203, 0.1736481776669307198 ) ) ;
#8306 = CARTESIAN_POINT ( 'NONE',  ( 5.000000000000000888, 0.000000000000000000, 0.000000000000000000 ) ) ;
#8307 = CYLINDRICAL_SURFACE ( 'NONE', #11077, 5.000000000000000000 ) ;
#8308 = ORIENTED_EDGE ( 'NONE', *, *, #7559, .F. ) ;
#8309 = FACE_BOUND ( 'NONE', #9058, .T. ) ;
#8310 = CARTESIAN_POINT ( 'NONE',  ( -21.75699517953123774, 54.99788995967445970, -0.006179814837821989357 ) ) ;
#8311 = CARTESIAN_POINT ( 'NONE',  ( -52.79756777621546604, 58.97512417236831794, 3.050472611213659313 ) ) ;
#8312 = CARTESIAN_POINT ( 'NONE',  ( 25.00000000000000000, 76.00000000000000000, 0.000000000000000000 ) ) ;
#8313 = CARTESIAN_POINT ( 'NONE',  ( -74.84375000409676204, 30.00000000000001421, 10.35533905932739174 ) ) ;
#8314 = CARTESIAN_POINT ( 'NONE',  ( -2.556751989345197984, 51.48122000982115765, -6.100625743585796457 ) ) ;
#8315 = EDGE_LOOP ( 'NONE', ( #1553, #6676, #11327, #1239 ) ) ;
#8316 = CARTESIAN_POINT ( 'NONE',  ( 14.85570562722353749, 52.25434861561973321, 21.02374011750137939 ) ) ;
#8317 = CARTESIAN_POINT ( 'NONE',  ( -72.03125000204838102, 55.00000000000000000, -25.81189881249999729 ) ) ;
#8318 = DIRECTION ( 'NONE',  ( -1.000000000000000000, 0.000000000000000000, 0.000000000000000000 ) ) ;
#8319 = CARTESIAN_POINT ( 'NONE',  ( 3.000000000000000000, 3.673940397442059868E-16, -4.346257142857142597 ) ) ;
#8320 = CARTESIAN_POINT ( 'NONE',  ( -72.87500000204839523, 65.69163855873949842, 25.81189881250000440 ) ) ;
#8321 = DIRECTION ( 'NONE',  ( 0.000000000000000000, 1.000000000000000000, 0.000000000000000000 ) ) ;
#8322 = PRESENTATION_LAYER_ASSIGNMENT (  '', '', ( #11181 ) ) ;
#8323 = ORIENTED_EDGE ( 'NONE', *, *, #9382, .F. ) ;
#8324 = CARTESIAN_POINT ( 'NONE',  ( -77.93750000204838102, 44.30836144126050158, -25.81189881249999374 ) ) ;
#8325 = ORIENTED_EDGE ( 'NONE', *, *, #2866, .F. ) ;
#8326 = CARTESIAN_POINT ( 'NONE',  ( 11.04711134339418876, 69.12045815601207721, -20.65175458094307004 ) ) ;
#8327 = CARTESIAN_POINT ( 'NONE',  ( -42.33147328884727045, 60.36255737924431486, -12.94746809434214541 ) ) ;
#8328 = CARTESIAN_POINT ( 'NONE',  ( -79.15625000204839523, 73.25176868561975141, -18.25176868561974430 ) ) ;
#8329 = CARTESIAN_POINT ( 'NONE',  ( -74.99999999999998579, 79.77762491170771852, 4.737166167340707723 ) ) ;
#8330 = ADVANCED_FACE ( 'NONE', ( #10479 ), #8931, .F. ) ;
#8331 = CARTESIAN_POINT ( 'NONE',  ( 0.000000000000000000, 0.000000000000000000, -0.02539999999999996774 ) ) ;
#8332 = ORIENTED_EDGE ( 'NONE', *, *, #2436, .T. ) ;
#8333 = DIRECTION ( 'NONE',  ( -1.000000000000000000, -0.000000000000000000, -0.000000000000000000 ) ) ;
#8334 = CARTESIAN_POINT ( 'NONE',  ( -71.34302368722833876, 77.35376350879521112, 12.90594348738575903 ) ) ;
#8335 = DIRECTION ( 'NONE',  ( -1.000000000000000000, 0.000000000000000000, 0.000000000000000000 ) ) ;
#8336 = FACE_BOUND ( 'NONE', #5613, .T. ) ;
#8337 = CARTESIAN_POINT ( 'NONE',  ( -59.46281197144560338, 55.00344839445808276, -0.006247678623671736216 ) ) ;
#8338 = APPLICATION_PROTOCOL_DEFINITION ( 'draft international standard', 'automotive_design', 1998, #11501 ) ;
#8339 = CARTESIAN_POINT ( 'NONE',  ( -17.99829699906814184, 73.95811728008973773, 11.16634296551433714 ) ) ;
#8340 = AXIS2_PLACEMENT_3D ( 'NONE', #7000, #2435, #8788 ) ;
#8341 = FACE_OUTER_BOUND ( 'NONE', #5684, .T. ) ;
#8342 = ORIENTED_EDGE ( 'NONE', *, *, #10730, .T. ) ;
#8343 = CARTESIAN_POINT ( 'NONE',  ( -79.71875000000000000, 79.99999999999998579, -10.35533905932736332 ) ) ;
#8344 = PRESENTATION_LAYER_ASSIGNMENT (  '', '', ( #8538 ) ) ;
#8345 = ADVANCED_FACE ( 'NONE', ( #865 ), #9592, .T. ) ;
#8346 = FACE_OUTER_BOUND ( 'NONE', #9050, .T. ) ;
#8347 = ORIENTED_EDGE ( 'NONE', *, *, #9461, .F. ) ;
#8348 = CARTESIAN_POINT ( 'NONE',  ( 2.003855453843550460, 35.57695044197526357, -8.044733130177707636 ) ) ;
#8349 = CARTESIAN_POINT ( 'NONE',  ( -77.09375000204839523, 55.00000000000000000, 25.81189881249999729 ) ) ;
#8350 = PRODUCT_DEFINITION_SHAPE ( 'NONE', 'NONE',  #11855 ) ;
#8351 = CARTESIAN_POINT ( 'NONE',  ( 5.000000000000000000, 2.419979747126330683, -0.3118366332702858790 ) ) ;
#8352 = CARTESIAN_POINT ( 'NONE',  ( -34.85572910849313644, 38.22605186251247744, -12.89098713163435228 ) ) ;
#8353 = CIRCLE ( 'NONE', #8171, 1.500000000000001332 ) ;
#8354 = B_SPLINE_CURVE_WITH_KNOTS ( 'NONE', 3,
 ( #3769, #7437, #4794, #11064, #5454, #10231, #8267, #10947, #2757, #3894, #10999, #7556, #6416, #1845, #9273, #165, #2875, #7500, #2935, #2025, #5513, #11179, #11124, #5699, #9160, #9337, #2811, #10106, #1906, #5574, #11475, #1310, #8741, #7613, #5761, #4124, #9398, #5822, #9459, #11242, #4074, #3053, #7731, #3951, #4976, #10293, #9579, #1193, #4857, #5094, #5038, #6723, #7787, #8685, #9635, #7847, #10523, #10354, #2151, #6895, #467, #1375, #11416, #6660, #3227, #1431, #2331, #346, #1245, #524, #6002, #4185 ),
 .UNSPECIFIED., .F., .F.,
 ( 4, 2, 2, 2, 2, 2, 2, 2, 2, 2, 2, 2, 2, 2, 2, 2, 2, 2, 2, 2, 2, 2, 2, 2, 2, 2, 2, 2, 2, 2, 2, 2, 2, 2, 2, 4 ),
 ( 0.1589808399053934673, 0.1602572277490322550, 0.1615336155926710426, 0.1628100034363098303, 0.1640863912799486179, 0.1666391669672261933, 0.1691919426545037686, 0.1717447183417813439, 0.1742974940290588914, 0.1794030454036140143, 0.1819558210908915896, 0.1832322089345303495, 0.1845085967781691372, 0.1896141481527242600, 0.1908905359963630199, 0.1921669238400018076, 0.1947196995272793552, 0.1972724752145569305, 0.1998252509018344780, 0.2011016387454732657, 0.2023780265891120256, 0.2049308022763896009, 0.2074835779636671484, 0.2100363536509446960, 0.2125891293382222713, 0.2138655171818610590, 0.2151419050254998466, 0.2202474564000549972, 0.2228002320873325726, 0.2253530077746101479, 0.2304585591491652985, 0.2330113348364428738, 0.2355641105237204491, 0.2368404983673592368, 0.2381168862109980244, 0.2406696618982755997 ),
 .UNSPECIFIED. ) ;
#8355 = EDGE_CURVE ( 'NONE', #6384, #10958, #789, .T. ) ;
#8356 = AXIS2_PLACEMENT_3D ( 'NONE', #8033, #11733, #5278 ) ;
#8357 = CARTESIAN_POINT ( 'NONE',  ( -65.17448922114576249, 36.67438677247554324, 10.54995967583099237 ) ) ;
#8358 = EDGE_LOOP ( 'NONE', ( #11222, #7909, #10484, #9164, #3130, #7914, #2287, #4560, #8832 ) ) ;
#8359 = CARTESIAN_POINT ( 'NONE',  ( -73.90625000204839523, 36.74823131438026280, 18.25176868561974786 ) ) ;
#8360 = CARTESIAN_POINT ( 'NONE',  ( -2.651582617587235458, 52.49162778365467830, -4.337637646355388732 ) ) ;
#8361 = CARTESIAN_POINT ( 'NONE',  ( -78.50000000000000000, 55.00000000000000000, -24.99999999999999645 ) ) ;
#8362 = ORIENTED_EDGE ( 'NONE', *, *, #8476, .F. ) ;
#8363 = CARTESIAN_POINT ( 'NONE',  ( -23.85572910907371025, 49.50876680309251299, 20.43178602932799492 ) ) ;
#8364 = AXIS2_PLACEMENT_3D ( 'NONE', #6568, #8473, #8528 ) ;
#8365 = CARTESIAN_POINT ( 'NONE',  ( -66.47562283042974229, 38.19906477560226676, 12.92409071120044040 ) ) ;
#8366 = PRESENTATION_STYLE_ASSIGNMENT (( #10273 ) ) ;
#8367 = AXIS2_PLACEMENT_3D ( 'NONE', #6331, #5420, #10793 ) ;
#8368 = EDGE_CURVE ( 'NONE', #2186, #11526, #6191, .T. ) ;
#8369 = FACE_OUTER_BOUND ( 'NONE', #5366, .T. ) ;
#8370 = CARTESIAN_POINT ( 'NONE',  ( -75.50000000409677625, 80.00000000000000000, -1.530808498934191324E-15 ) ) ;
#8371 = ORIENTED_EDGE ( 'NONE', *, *, #9746, .T. ) ;
#8372 =( BOUNDED_CURVE ( )  B_SPLINE_CURVE ( 2, ( #6041, #3994, #9677, #10335, #451, #5805, #7654, #9439, #1228 ),
 .UNSPECIFIED., .F., .T. ) 
 B_SPLINE_CURVE_WITH_KNOTS ( ( 3, 2, 2, 2, 3 ),
 ( 0.07919667986333785159, 0.09899957127346223351, 0.1188024626835866154, 0.1386053540937109974, 0.1584082455038353654 ),
 .UNSPECIFIED. ) 
 CURVE ( )  GEOMETRIC_REPRESENTATION_ITEM ( )  RATIONAL_B_SPLINE_CURVE ( ( 0.9999999999999998890, 0.9238795325112866275, 0.9999999999999998890, 0.9238795325112866275, 0.9999999999999998890, 0.9238795325112866275, 0.9999999999999998890, 0.9238795325113071666, 0.9999999999999793499 ) ) 
 REPRESENTATION_ITEM ( '' )  );
#8373 = CARTESIAN_POINT ( 'NONE',  ( -79.43750000000001421, 72.67766952966368876, 17.67766952966368521 ) ) ;
#8374 = CARTESIAN_POINT ( 'NONE',  ( -23.49650511202184688, 55.00077215910898332, 0.002398592362466134536 ) ) ;
#8375 = CARTESIAN_POINT ( 'NONE',  ( -42.68304982271171610, 57.50651106462216688, -4.338678109911903391 ) ) ;
#8376 = CARTESIAN_POINT ( 'NONE',  ( -77.18750000000007105, 37.32233047033638229, -17.67766952966361771 ) ) ;
#8377 = FACE_BOUND ( 'NONE', #8840, .T. ) ;
#8378 = CARTESIAN_POINT ( 'NONE',  ( 1.333197741078869125, 48.52671685189832829, -2.680978973290799150 ) ) ;
#8379 = ORIENTED_EDGE ( 'NONE', *, *, #9813, .F. ) ;
#8380 = CARTESIAN_POINT ( 'NONE',  ( 24.18742635297404675, 76.02379904146428657, 2.751050496637376774 ) ) ;
#8381 = UNCERTAINTY_MEASURE_WITH_UNIT (LENGTH_MEASURE( 1.000000000000000082E-05 ), #3391, 'distance_accuracy_value', 'NONE');
#8382 =( REPRESENTATION_RELATIONSHIP ('NONE','NONE', #5489, #3715 ) REPRESENTATION_RELATIONSHIP_WITH_TRANSFORMATION ( #7337 )SHAPE_REPRESENTATION_RELATIONSHIP( ) );
#8383 = LINE ( 'NONE', #8624, #7297 ) ;
#8384 = DIRECTION ( 'NONE',  ( 0.000000000000000000, 0.000000000000000000, 1.000000000000000000 ) ) ;
#8385 = CARTESIAN_POINT ( 'NONE',  ( 3.744923233462341604E-15, 110.0000000000000000, -30.57961884250791940 ) ) ;
#8386 = DIRECTION ( 'NONE',  ( 0.000000000000000000, 1.000000000000000000, 0.000000000000000000 ) ) ;
#8387 = CARTESIAN_POINT ( 'NONE',  ( -78.78125000204839523, 73.25176868561975141, 18.25176868561974075 ) ) ;
#8388 = AXIS2_PLACEMENT_3D ( 'NONE', #9758, #8695, #534 ) ;
#8389 = VERTEX_POINT ( 'NONE', #6909 ) ;
#8390 = CARTESIAN_POINT ( 'NONE',  ( -75.96875000204839523, 80.81189881250000440, -1.580522963032174394E-15 ) ) ;
#8391 = ORIENTED_EDGE ( 'NONE', *, *, #5286, .T. ) ;
#8392 = CARTESIAN_POINT ( 'NONE',  ( 25.29007368494098884, 80.00022686158581564, -0.4132073972999723566 ) ) ;
#8393 = CARTESIAN_POINT ( 'NONE',  ( -62.17173789034691112, 47.18625706333304493, 11.70555309606978689 ) ) ;
#8394 = CARTESIAN_POINT ( 'NONE',  ( -71.34302368722835297, 77.35376350879521112, 12.90594348738575903 ) ) ;
#8395 = FACE_BOUND ( 'NONE', #988, .T. ) ;
#8396 = CARTESIAN_POINT ( 'NONE',  ( 39.99999999999999289, 55.00000000000000000, 0.000000000000000000 ) ) ;
#8397 = ORIENTED_EDGE ( 'NONE', *, *, #11561, .F. ) ;
#8398 = LINE ( 'NONE', #10062, #3813 ) ;
#8399 = CARTESIAN_POINT ( 'NONE',  ( -76.25000000409677625, 30.00000000000000355, 4.592425496802573578E-15 ) ) ;
#8400 = CARTESIAN_POINT ( 'NONE',  ( -34.73940033462148591, 50.06485160516485422, -0.8190406228260763699 ) ) ;
#8401 = DIRECTION ( 'NONE',  ( -0.000000000000000000, -0.000000000000000000, -1.000000000000000000 ) ) ;
#8402 = EDGE_CURVE ( 'NONE', #9331, #5852, #8650, .T. ) ;
#8403 = CARTESIAN_POINT ( 'NONE',  ( -6.417135814581119035, 59.43955965505210060, -5.410182326209246106 ) ) ;
#8404 = CARTESIAN_POINT ( 'NONE',  ( -14.41642088558921486, 71.22858682633147964, 14.86374956074409681 ) ) ;
#8405 = CIRCLE ( 'NONE', #5533, 4.999999999999995559 ) ;
#8406 = DIRECTION ( 'NONE',  ( 0.000000000000000000, -0.7071067811865441310, -0.7071067811865507924 ) ) ;
#8407 = EDGE_LOOP ( 'NONE', ( #6025, #6751, #10396, #6183 ) ) ;
#8408 = CARTESIAN_POINT ( 'NONE',  ( 62.44550000000000267, 55.00000000000000000, 0.000000000000000000 ) ) ;
#8409 = CARTESIAN_POINT ( 'NONE',  ( 1.034159948410326981E-15, 5.773502691896260863, -6.099999999999999645 ) ) ;
#8410 = EDGE_CURVE ( 'NONE', #5247, #10943, #7088, .T. ) ;
#8411 = ORIENTED_EDGE ( 'NONE', *, *, #5783, .T. ) ;
#8412 = CARTESIAN_POINT ( 'NONE',  ( -68.86034823945129801, 34.02049636744572325, 2.749403782478469616 ) ) ;
#8413 = CARTESIAN_POINT ( 'NONE',  ( -72.68750000204839523, 44.30836144126053000, 25.81189881250000795 ) ) ;
#8414 = AXIS2_PLACEMENT_3D ( 'NONE', #11047, #3816, #7484 ) ;
#8415 = VECTOR ( 'NONE', #9089, 1000.000000000000000 ) ;
#8416 = DIRECTION ( 'NONE',  ( 0.000000000000000000, 0.000000000000000000, 1.000000000000000000 ) ) ;
#8417 = CARTESIAN_POINT ( 'NONE',  ( -52.59603425219209782, 73.55155261293346314, 9.913157997185967574 ) ) ;
#8418 = SURFACE_STYLE_FILL_AREA ( #10205 ) ;
#8419 = CARTESIAN_POINT ( 'NONE',  ( -53.45210586504737904, 71.88419113761085555, 12.52116934359859002 ) ) ;
#8420 = EDGE_LOOP ( 'NONE', ( #7045, #2162, #5924, #9018 ) ) ;
#8421 = CARTESIAN_POINT ( 'NONE',  ( -72.21875000204838102, 29.18810118750000271, 4.741568889096522788E-15 ) ) ;
#8422 = CARTESIAN_POINT ( 'NONE',  ( -11.20418418299178320, 58.97469996104722156, -3.050991650916503595 ) ) ;
#8423 = DIRECTION ( 'NONE',  ( -1.000000000000000000, 0.000000000000000000, 0.000000000000000000 ) ) ;
#8424 = VERTEX_POINT ( 'NONE', #653 ) ;
#8425 = EDGE_CURVE ( 'NONE', #301, #3293, #5161, .T. ) ;
#8426 = CARTESIAN_POINT ( 'NONE',  ( -33.39182374990940616, 34.82582084984149873, -6.127586950986167125 ) ) ;
#8427 = CARTESIAN_POINT ( 'NONE',  ( -52.82691659388441252, 75.69008924411679118, 4.122156975067814422 ) ) ;
#8428 = DIRECTION ( 'NONE',  ( 0.000000000000000000, 0.000000000000000000, 1.000000000000000000 ) ) ;
#8429 = CARTESIAN_POINT ( 'NONE',  ( 14.99999999999999645, -30.00000000000000000, -10.00000000000000000 ) ) ;
#8430 = CIRCLE ( 'NONE', #1150, 2.500000000000000000 ) ;
#8431 = CARTESIAN_POINT ( 'NONE',  ( 0.000000000000000000, 0.000000000000000000, -0.3755037691048591086 ) ) ;
#8432 = VERTEX_POINT ( 'NONE', #2396 ) ;
#8433 = CARTESIAN_POINT ( 'NONE',  ( -75.50000000000000000, 55.00000000000000000, -24.99999999999999645 ) ) ;
#8434 = CARTESIAN_POINT ( 'NONE',  ( -16.09272391817585657, 55.01637097774587204, 0.001658295702028558935 ) ) ;
#8435 = CARTESIAN_POINT ( 'NONE',  ( -48.12550986829561595, 59.96676360895955327, -0.6610507428945817665 ) ) ;
#8436 = ADVANCED_FACE ( 'NONE', ( #6854 ), #9761, .T. ) ;
#8437 = EDGE_CURVE ( 'NONE', #5411, #7145, #6417, .T. ) ;
#8438 = DIRECTION ( 'NONE',  ( -0.000000000000000000, -1.000000000000000000, -0.000000000000000000 ) ) ;
#8439 = EDGE_CURVE ( 'NONE', #9870, #11, #4261, .T. ) ;
#8440 = AXIS2_PLACEMENT_3D ( 'NONE', #8980, #7790, #3230 ) ;
#8441 = CIRCLE ( 'NONE', #3088, 3.000000000000000888 ) ;
#8442 = CARTESIAN_POINT ( 'NONE',  ( -78.00000000000001421, 59.24264068711927678, 4.242644059037073312 ) ) ;
#8443 = CARTESIAN_POINT ( 'NONE',  ( -1.776549974196238946, 50.68601013462039617, -5.609814685327735972 ) ) ;
#8444 = VERTEX_POINT ( 'NONE', #480 ) ;
#8445 = CARTESIAN_POINT ( 'NONE',  ( 0.000000000000000000, 0.000000000000000000, -4.696360911962001339 ) ) ;
#8446 = DIRECTION ( 'NONE',  ( 0.000000000000000000, -0.000000000000000000, 1.000000000000000000 ) ) ;
#8447 = DIRECTION ( 'NONE',  ( -1.000000000000000000, 0.000000000000000000, 0.000000000000000000 ) ) ;
#8448 = CARTESIAN_POINT ( 'NONE',  ( -80.00000000000001421, 46.51471862576140381, -8.485278002320759683 ) ) ;
#8449 =( BOUNDED_CURVE ( )  B_SPLINE_CURVE ( 2, ( #9350, #9286, #11197, #10305, #11079, #1922, #3007, #7386, #6677 ),
 .UNSPECIFIED., .F., .T. ) 
 B_SPLINE_CURVE_WITH_KNOTS ( ( 3, 2, 2, 2, 3 ),
 ( 0.5545069179274292326, 0.5743159892607880845, 0.5941250605941470475, 0.6139341319275060105, 0.6337432032608648624 ),
 .UNSPECIFIED. ) 
 CURVE ( )  GEOMETRIC_REPRESENTATION_ITEM ( )  RATIONAL_B_SPLINE_CURVE ( ( 1.000000000000015321, 0.9238795325112713064, 1.000000000000000000, 0.9238795325112867385, 1.000000000000000000, 0.9238795325112867385, 1.000000000000000000, 0.9238795325112867385, 1.000000000000000000 ) ) 
 REPRESENTATION_ITEM ( '' )  );
#8450 = CARTESIAN_POINT ( 'NONE',  ( -72.03125000204838102, 55.00000000000000000, -25.81189881249999729 ) ) ;
#8451 = CARTESIAN_POINT ( 'NONE',  ( -72.21875000204838102, 36.74823131438024859, -18.25176868561973720 ) ) ;
#8452 = ORIENTED_EDGE ( 'NONE', *, *, #7989, .T. ) ;
#8453 = CARTESIAN_POINT ( 'NONE',  ( -77.18750000409679046, 72.67766952966368876, -17.67766952966368876 ) ) ;
#8454 = AXIS2_PLACEMENT_3D ( 'NONE', #9042, #3702, #11728 ) ;
#8455 = AXIS2_PLACEMENT_3D ( 'NONE', #6266, #10851, #5299 ) ;
#8456 = EDGE_LOOP ( 'NONE', ( #2784, #7201 ) ) ;
#8457 = CARTESIAN_POINT ( 'NONE',  ( 24.47797982529632321, 79.30575909152375402, -5.865156235303714993 ) ) ;
#8458 = CARTESIAN_POINT ( 'NONE',  ( -47.79377051319855241, 68.65769002727881798, -3.675352279733770544 ) ) ;
#8459 = VECTOR ( 'NONE', #1436, 1000.000000000000000 ) ;
#8460 = CARTESIAN_POINT ( 'NONE',  ( -79.06250000204839523, 80.81189881250000440, 10.69163855873948243 ) ) ;
#8461 = CARTESIAN_POINT ( 'NONE',  ( -74.99999999999998579, 76.80627241285399975, -13.27287850887629084 ) ) ;
#8462 = CARTESIAN_POINT ( 'NONE',  ( -4.067038661182964928E-21, 64.99605696851786263, 19.59792961213366169 ) ) ;
#8463 = VECTOR ( 'NONE', #3257, 1000.000000000000000 ) ;
#8464 = ORIENTED_EDGE ( 'NONE', *, *, #4044, .F. ) ;
#8465 = DIRECTION ( 'NONE',  ( 0.000000000000000000, 1.000000000000000000, 0.000000000000000000 ) ) ;
#8466 = CARTESIAN_POINT ( 'NONE',  ( -78.00000000000001421, 67.72792206135787296, 4.242644059037073312 ) ) ;
#8467 = CARTESIAN_POINT ( 'NONE',  ( -71.38989868722833876, 77.35376350879521112, 12.90594348738575903 ) ) ;
#8468 = DIRECTION ( 'NONE',  ( -1.000000000000000000, -0.000000000000000000, -0.000000000000000000 ) ) ;
#8469 = CARTESIAN_POINT ( 'NONE',  ( -18.08380248123574319, 58.29941079146190930, 6.172005441165978823 ) ) ;
#8470 = CARTESIAN_POINT ( 'NONE',  ( 62.44550000000000267, 55.00000000000000000, -2.999999999999995559 ) ) ;
#8471 = DIRECTION ( 'NONE',  ( 0.000000000000000000, 0.000000000000000000, -1.000000000000000000 ) ) ;
#8472 = ORIENTED_EDGE ( 'NONE', *, *, #10909, .F. ) ;
#8473 = DIRECTION ( 'NONE',  ( 1.000000000000000000, 6.033820786006286457E-17, -0.000000000000000000 ) ) ;
#8474 = CARTESIAN_POINT ( 'NONE',  ( -73.81250000409677625, 72.67766952966368876, 17.67766952966368521 ) ) ;
#8475 = VERTEX_POINT ( 'NONE', #5226 ) ;
#8476 = EDGE_CURVE ( 'NONE', #1618, #10685, #8838, .T. ) ;
#8477 = CARTESIAN_POINT ( 'NONE',  ( -43.21475900837984341, 58.08538667521604282, -20.80084980650556759 ) ) ;
#8478 = CARTESIAN_POINT ( 'NONE',  ( -72.78125000204839523, 73.25176868561975141, 18.25176868561974075 ) ) ;
#8479 = CARTESIAN_POINT ( 'NONE',  ( 5.000000000000000000, 2.886751345948134428, -0.4465819873852071575 ) ) ;
#8480 = CARTESIAN_POINT ( 'NONE',  ( -50.27495406422890767, 76.01781437481966464, 2.059423474151367728 ) ) ;
#8481 = SHAPE_REPRESENTATION_RELATIONSHIP ( 'NONE' , 'NONE' ,  #4172, #4566 ) ;
#8482 = DIRECTION ( 'NONE',  ( -1.000000000000000000, -0.000000000000000000, -0.000000000000000000 ) ) ;
#8483 = ORIENTED_EDGE ( 'NONE', *, *, #3463, .F. ) ;
#8484 = B_SPLINE_CURVE_WITH_KNOTS ( 'NONE', 1,
 ( #1104, #2915 ),
 .UNSPECIFIED., .F., .F.,
 ( 2, 2 ),
 ( 0.000000000000000000, 1.000000000000000000 ),
 .UNSPECIFIED. ) ;
#8485 = CARTESIAN_POINT ( 'NONE',  ( -71.65625000204839523, 73.25176868561975141, -18.25176868561974430 ) ) ;
#8486 = CARTESIAN_POINT ( 'NONE',  ( -9.656863044840665822, 58.05255974435234378, -3.973617159649989183 ) ) ;
#8487 = CARTESIAN_POINT ( 'NONE',  ( 17.52230480588388417, 67.92092721363508190, 16.80419350660125843 ) ) ;
#8488 = ORIENTED_EDGE ( 'NONE', *, *, #6057, .T. ) ;
#8489 = CARTESIAN_POINT ( 'NONE',  ( -21.72515708326280048, 57.05917195472675019, 20.98343720861656436 ) ) ;
#8490 = CARTESIAN_POINT ( 'NONE',  ( -63.63584090060282961, 46.00639722032484968, 19.01118640546643590 ) ) ;
#8491 = DIRECTION ( 'NONE',  ( -1.000000000000000000, 0.000000000000000000, 0.000000000000000000 ) ) ;
#8492 = DIRECTION ( 'NONE',  ( 0.000000000000000000, 1.000000000000000000, 0.000000000000000000 ) ) ;
#8493 = CARTESIAN_POINT ( 'NONE',  ( -79.43750000204838102, 55.00000000000000000, -24.99999999999999645 ) ) ;
#8494 = CARTESIAN_POINT ( 'NONE',  ( 36.99999999999999289, 55.00000000000000000, 0.000000000000000000 ) ) ;
#8495 = VERTEX_POINT ( 'NONE', #1443 ) ;
#8496 = CARTESIAN_POINT ( 'NONE',  ( -78.87500000000000000, 30.00000000000000355, 4.592425496802573578E-15 ) ) ;
#8497 = CARTESIAN_POINT ( 'NONE',  ( -67.42686117391447453, 54.98684645604348020, 0.008483758310626438731 ) ) ;
#8498 = FACE_OUTER_BOUND ( 'NONE', #3526, .T. ) ;
#8499 = CARTESIAN_POINT ( 'NONE',  ( 14.99999999999999645, 5.000000000000000000, -29.99999999999999289 ) ) ;
#8500 = CARTESIAN_POINT ( 'NONE',  ( 3.666806354490720565, 47.98949887324683061, -0.0002676899127992829822 ) ) ;
#8501 = ORIENTED_EDGE ( 'NONE', *, *, #7023, .F. ) ;
#8502 = CARTESIAN_POINT ( 'NONE',  ( -5.337209886265139147, 63.04750289227570192, -19.42727033598380970 ) ) ;
#8503 = DIRECTION ( 'NONE',  ( 0.000000000000000000, 1.000000000000000000, 0.000000000000000000 ) ) ;
#8504 = EDGE_CURVE ( 'NONE', #6038, #10429, #4137, .T. ) ;
#8505 = DIRECTION ( 'NONE',  ( -0.000000000000000000, -0.000000000000000000, 1.000000000000000000 ) ) ;
#8506 = CARTESIAN_POINT ( 'NONE',  ( 4.350743830703725834, 50.03278576500255070, 0.6577445178750861432 ) ) ;
#8507 = DIRECTION ( 'NONE',  ( -0.000000000000000000, -1.000000000000000000, -0.000000000000000000 ) ) ;
#8508 = CARTESIAN_POINT ( 'NONE',  ( -77.75000000204839523, 65.69163855873948421, -25.81189881250000440 ) ) ;
#8509 = VERTEX_POINT ( 'NONE', #6014 ) ;
#8510 = CARTESIAN_POINT ( 'NONE',  ( -73.90625000204839523, 36.74823131438026280, 18.25176868561974786 ) ) ;
#8511 = CARTESIAN_POINT ( 'NONE',  ( -78.12500000409677625, 55.00000000000000000, 24.99999999999999645 ) ) ;
#8512 = CARTESIAN_POINT ( 'NONE',  ( 8.878302819564396486, 67.93238317198033371, -21.39628370427902126 ) ) ;
#8513 = CARTESIAN_POINT ( 'NONE',  ( 24.18742635297404675, 76.02379904146428657, 2.751050496637376774 ) ) ;
#8514 = EDGE_CURVE ( 'NONE', #3681, #8959, #5846, .T. ) ;
#8515 = DIRECTION ( 'NONE',  ( -0.000000000000000000, -0.000000000000000000, -1.000000000000000000 ) ) ;
#8516 = CARTESIAN_POINT ( 'NONE',  ( -74.99999999999998579, 78.53260953835976466, -9.507204588591818606 ) ) ;
#8517 = LINE ( 'NONE', #300, #4374 ) ;
#8518 = COLOUR_RGB ( '',0.8941176470588234615, 0.8941176470588234615, 0.8941176470588234615 ) ;
#8519 = ORIENTED_EDGE ( 'NONE', *, *, #6101, .T. ) ;
#8520 = CARTESIAN_POINT ( 'NONE',  ( -75.78125000000001421, 30.00000000000000355, -10.35533905932738108 ) ) ;
#8521 = CARTESIAN_POINT ( 'NONE',  ( -74.93750000409677625, 37.32233047033631124, 17.67766952966369232 ) ) ;
#8522 = FACE_OUTER_BOUND ( 'NONE', #5379, .T. ) ;
#8523 = ORIENTED_EDGE ( 'NONE', *, *, #10549, .T. ) ;
#8524 = CARTESIAN_POINT ( 'NONE',  ( -17.20817491345679784, 59.17780944700501777, 5.632517163406045135 ) ) ;
#8525 = CARTESIAN_POINT ( 'NONE',  ( -13.90763988834204135, 70.86184651638554044, 15.25345997699037426 ) ) ;
#8526 = DIRECTION ( 'NONE',  ( 0.000000000000000000, 0.000000000000000000, -1.000000000000000000 ) ) ;
#8527 = ORIENTED_EDGE ( 'NONE', *, *, #4691, .T. ) ;
#8528 = DIRECTION ( 'NONE',  ( 0.000000000000000000, 1.000000000000000000, 0.000000000000000000 ) ) ;
#8529 = CARTESIAN_POINT ( 'NONE',  ( -78.40625000204838102, 29.18810118750000271, 4.741568889096522788E-15 ) ) ;
#8530 = VERTEX_POINT ( 'NONE', #3182 ) ;
#8531 = EDGE_CURVE ( 'NONE', #5005, #3681, #11254, .T. ) ;
#8532 = CARTESIAN_POINT ( 'NONE',  ( -61.88037028687247698, 51.91449295574040690, 20.80032498971814192 ) ) ;
#8533 = CARTESIAN_POINT ( 'NONE',  ( -71.75000000204840944, 65.69163855873948421, -25.81189881250000440 ) ) ;
#8534 = CIRCLE ( 'NONE', #3745, 30.57961884250791940 ) ;
#8535 = CARTESIAN_POINT ( 'NONE',  ( -2.500000000000000000, 3.061616997868383141E-16, -2.968018054819144158 ) ) ;
#8536 = DIRECTION ( 'NONE',  ( -1.000000000000000000, -0.000000000000000000, -0.000000000000000000 ) ) ;
#8537 = CARTESIAN_POINT ( 'NONE',  ( -77.65625000409676204, 30.00000000000000355, -10.35533905932738108 ) ) ;
#8538=STYLED_ITEM('',(#11902),#8858);
#8539 = EDGE_LOOP ( 'NONE', ( #4286, #11538 ) ) ;
#8540 = CARTESIAN_POINT ( 'NONE',  ( -71.34302368722833876, 77.35376350879521112, 12.90594348738575903 ) ) ;
#8541 = CARTESIAN_POINT ( 'NONE',  ( 53.00000000000004974, 4.648349522099639420E-14, 0.000000000000000000 ) ) ;
#8542 = CARTESIAN_POINT ( 'NONE',  ( 22.18771278451687579, 76.01886845420673922, 2.750080521686579793 ) ) ;
#8543 = AXIS2_PLACEMENT_3D ( 'NONE', #1348, #1406, #7587 ) ;
#8544 = EDGE_LOOP ( 'NONE', ( #9778, #6102, #3477, #3443 ) ) ;
#8545 = CARTESIAN_POINT ( 'NONE',  ( -60.54703689898057206, 51.91451759569049784, 20.80086399049218215 ) ) ;
#8546 = CARTESIAN_POINT ( 'NONE',  ( -53.69727390230763575, 74.79022971164903311, 7.081167078663678893 ) ) ;
#8547 = LINE ( 'NONE', #11397, #7853 ) ;
#8548 = CARTESIAN_POINT ( 'NONE',  ( 53.00000000000000000, 51.46446609406726935, 3.535533905932731091 ) ) ;
#8549 = EDGE_CURVE ( 'NONE', #7933, #1507, #6221, .T. ) ;
#8550 = AXIS2_PLACEMENT_3D ( 'NONE', #7796, #4986, #2275 ) ;
#8551 = CARTESIAN_POINT ( 'NONE',  ( -78.00000000000002842, 42.27207793864211283, -4.242637315201479353 ) ) ;
#8552 = CARTESIAN_POINT ( 'NONE',  ( 39.99999999999999289, 55.00000000000000000, 24.99999999999999645 ) ) ;
#8553 = EDGE_LOOP ( 'NONE', ( #8129, #11575 ) ) ;
#8554 = CARTESIAN_POINT ( 'NONE',  ( -75.68750000000000000, 37.32233047033631124, -17.67766952966368166 ) ) ;
#8555 = CARTESIAN_POINT ( 'NONE',  ( -75.00000000000001421, 58.46699551781524917, -25.57799957749213604 ) ) ;
#8556 = LINE ( 'NONE', #8312, #9921 ) ;
#8557 = AXIS2_PLACEMENT_3D ( 'NONE', #7580, #11206, #10664 ) ;
#8558 = DIRECTION ( 'NONE',  ( -0.000000000000000000, -0.000000000000000000, -1.000000000000000000 ) ) ;
#8559 = CARTESIAN_POINT ( 'NONE',  ( -4.890012301214623491, 54.08359342507363721, -6.982820483012029733 ) ) ;
#8560 = CIRCLE ( 'NONE', #3385, 2.500000000000000000 ) ;
#8561 = VERTEX_POINT ( 'NONE', #7358 ) ;
#8562 = CARTESIAN_POINT ( 'NONE',  ( -17.59602449223222109, 68.34579465778965357, 16.25793134507749826 ) ) ;
#8563 = CARTESIAN_POINT ( 'NONE',  ( -20.00000000000003197, -63.00000000000000000, -5.000000000000000000 ) ) ;
#8564 = EDGE_CURVE ( 'NONE', #11498, #3514, #4714, .T. ) ;
#8565 = CARTESIAN_POINT ( 'NONE',  ( -78.00000000000001421, 67.72792206135787296, -12.72791868944004534 ) ) ;
#8566 = DIRECTION ( 'NONE',  ( -0.000000000000000000, -0.000000000000000000, -1.000000000000000000 ) ) ;
#8567 = LINE ( 'NONE', #4013, #9928 ) ;
#8568 = CARTESIAN_POINT ( 'NONE',  ( -77.09375000204839523, 55.00000000000000000, 25.81189881249999729 ) ) ;
#8569 = ORIENTED_EDGE ( 'NONE', *, *, #9953, .F. ) ;
#8570 = VECTOR ( 'NONE', #8045, 1000.000000000000000 ) ;
#8571 = CARTESIAN_POINT ( 'NONE',  ( -78.87500000409677625, 55.00000000000000000, -24.99999999999999645 ) ) ;
#8572 = CARTESIAN_POINT ( 'NONE',  ( -75.68750000000005684, 37.32233047033638940, -17.67766952966360705 ) ) ;
#8573 = CARTESIAN_POINT ( 'NONE',  ( 23.34710263473544245, 78.34793618746451216, -8.970954660865723795 ) ) ;
#8574 = AXIS2_PLACEMENT_3D ( 'NONE', #3677, #11752, #2727 ) ;
#8575 = CARTESIAN_POINT ( 'NONE',  ( -57.49717384800269571, 57.74002937887566844, 13.79287161986824017 ) ) ;
#8576 = EDGE_CURVE ( 'NONE', #7948, #241, #3570, .T. ) ;
#8577 = FACE_OUTER_BOUND ( 'NONE', #6901, .T. ) ;
#8578 = DIRECTION ( 'NONE',  ( -0.000000000000000000, -1.000000000000000000, -0.000000000000000000 ) ) ;
#8579 = CARTESIAN_POINT ( 'NONE',  ( -80.00000000000001421, 67.72792206135787296, 4.242644059037073312 ) ) ;
#8580 = ADVANCED_FACE ( 'NONE', ( #6522 ), #10032, .F. ) ;
#8581 = CIRCLE ( 'NONE', #9714, 3.000000000000000000 ) ;
#8582 = ORIENTED_EDGE ( 'NONE', *, *, #10300, .T. ) ;
#8583 = EDGE_CURVE ( 'NONE', #1747, #7962, #10364, .T. ) ;
#8584 = EDGE_CURVE ( 'NONE', #9858, #11030, #8928, .T. ) ;
#8585 = CARTESIAN_POINT ( 'NONE',  ( -74.65625000000000000, 44.64466094067262958, 25.00000000000001066 ) ) ;
#8586 = CARTESIAN_POINT ( 'NONE',  ( -71.09375000409677625, 80.00000000000001421, -10.35533905932737753 ) ) ;
#8587 = MANIFOLD_SOLID_BREP ( 'Fill Pattern1', #11497 ) ;
#8588 = CARTESIAN_POINT ( 'NONE',  ( -79.53125000204838102, 55.00000000000000000, -25.81189881249999729 ) ) ;
#8589 = EDGE_LOOP ( 'NONE', ( #9342, #2888, #9816, #549 ) ) ;
#8590 = CARTESIAN_POINT ( 'NONE',  ( 21.77666841074465864, 60.57982234150205869, 4.283804165148911380 ) ) ;
#8591 = EDGE_CURVE ( 'NONE', #9929, #8651, #86, .T. ) ;
#8592 = ADVANCED_FACE ( 'NONE', ( #4593 ), #6584, .F. ) ;
#8593 = CARTESIAN_POINT ( 'NONE',  ( -72.87500000000007105, 30.00000000000014211, 4.592425496802547545E-15 ) ) ;
#8594 =( LENGTH_UNIT ( ) NAMED_UNIT ( * ) SI_UNIT ( .MILLI., .METRE. ) );
#8595 = EDGE_CURVE ( 'NONE', #5658, #9917, #2225, .T. ) ;
#8596 = EDGE_LOOP ( 'NONE', ( #6867, #1121, #1397, #7746 ) ) ;
#8597 = DIRECTION ( 'NONE',  ( -0.8191520442889885789, 1.003171929053520802E-16, 0.5735764363510507113 ) ) ;
#8598 = CARTESIAN_POINT ( 'NONE',  ( -76.25000000204838102, 80.81189881250000440, -10.69163855873948954 ) ) ;
#8599 = ORIENTED_EDGE ( 'NONE', *, *, #5431, .F. ) ;
#8600 = CARTESIAN_POINT ( 'NONE',  ( -57.50627882723209439, 66.73110044028416610, 17.54296274220338958 ) ) ;
#8601 = CARTESIAN_POINT ( 'NONE',  ( -71.34302368722833876, 77.35376350879521112, 12.90594348738575903 ) ) ;
#8602 = DIRECTION ( 'NONE',  ( 0.000000000000000000, 1.000000000000000000, 0.000000000000000000 ) ) ;
#8603 = DIRECTION ( 'NONE',  ( -0.04699449999129696326, 0.9988950444178830157, -0.0004552010143329844735 ) ) ;
#8604 = AXIS2_PLACEMENT_3D ( 'NONE', #11099, #7478, #3030 ) ;
#8605 = DIRECTION ( 'NONE',  ( 0.000000000000000000, 0.000000000000000000, -1.000000000000000000 ) ) ;
#8606 = ORIENTED_EDGE ( 'NONE', *, *, #7340, .T. ) ;
#8607 = CARTESIAN_POINT ( 'NONE',  ( -73.81250000204839523, 29.18810118750000981, 10.69163855873950020 ) ) ;
#8608 = CARTESIAN_POINT ( 'NONE',  ( 0.000000000000000000, 5.773502691896260863, -0.4465819873852071575 ) ) ;
#8609 = CARTESIAN_POINT ( 'NONE',  ( -8.785358865379802040, 67.52185545713140868, -16.88477868139494831 ) ) ;
#8610 = ORIENTED_EDGE ( 'NONE', *, *, #4766, .T. ) ;
#8611 = CARTESIAN_POINT ( 'NONE',  ( 19.81102887321632622, 71.77647403800290249, 12.89307786291128899 ) ) ;
#8612 = VECTOR ( 'NONE', #5922, 1000.000000000000000 ) ;
#8613 = CARTESIAN_POINT ( 'NONE',  ( 1.668526597461617023, 42.05183364693759529, -5.362856051735069407 ) ) ;
#8614 = DIRECTION ( 'NONE',  ( -0.000000000000000000, -1.000000000000000000, -0.000000000000000000 ) ) ;
#8615 = CARTESIAN_POINT ( 'NONE',  ( -76.43750000409679046, 37.32233047033631124, 17.67766952966369232 ) ) ;
#8616 = LINE ( 'NONE', #1359, #4582 ) ;
#8617 = ORIENTED_EDGE ( 'NONE', *, *, #8066, .T. ) ;
#8618 = CARTESIAN_POINT ( 'NONE',  ( -76.43750000000000000, 72.67766952966368876, 17.67766952966368521 ) ) ;
#8619 = CARTESIAN_POINT ( 'NONE',  ( -20.00000000000003197, -63.00000000000000000, 5.000000000000000000 ) ) ;
#8620 = CARTESIAN_POINT ( 'NONE',  ( -5.000000000000000000, -2.886751345948134428, -0.4465819873852071575 ) ) ;
#8621 = CARTESIAN_POINT ( 'NONE',  ( -19.37536588012664041, 60.18888662840161885, 4.702399783581789450 ) ) ;
#8622 = ORIENTED_EDGE ( 'NONE', *, *, #5148, .T. ) ;
#8623 = CARTESIAN_POINT ( 'NONE',  ( -52.88146049032556562, 73.03766007303350705, 10.81102556547625149 ) ) ;
#8624 = CARTESIAN_POINT ( 'NONE',  ( 47.00000000000000000, 51.46446609406726935, -3.535533905932738197 ) ) ;
#8625 = LINE ( 'NONE', #5036, #5634 ) ;
#8626 = CARTESIAN_POINT ( 'NONE',  ( -76.53125000204839523, 36.74823131438024859, -18.25176868561973720 ) ) ;
#8627 = EDGE_CURVE ( 'NONE', #5840, #10958, #2049, .T. ) ;
#8628 = CARTESIAN_POINT ( 'NONE',  ( -76.15625000000005684, 44.64466094067266511, 24.99999999999990408 ) ) ;
#8629 = CARTESIAN_POINT ( 'NONE',  ( -73.34375000204839523, 73.25176868561975141, -18.25176868561974430 ) ) ;
#8630 = VECTOR ( 'NONE', #11144, 1000.000000000000000 ) ;
#8631 = VERTEX_POINT ( 'NONE', #3014 ) ;
#8632 = CARTESIAN_POINT ( 'NONE',  ( -72.31250000204839523, 29.18810118750000981, 10.69163855873950020 ) ) ;
#8633 = ORIENTED_EDGE ( 'NONE', *, *, #741, .T. ) ;
#8634 = CARTESIAN_POINT ( 'NONE',  ( -7.969360823174009845, 70.58422527244209732, -14.12522777056770629 ) ) ;
#8635 = AXIS2_PLACEMENT_3D ( 'NONE', #7422, #2073, #11048 ) ;
#8636 = PLANE ( 'NONE',  #8248 ) ;
#8637 = FACE_BOUND ( 'NONE', #10004, .T. ) ;
#8638 = AXIS2_PLACEMENT_3D ( 'NONE', #5758, #11359, #3113 ) ;
#8639 = CARTESIAN_POINT ( 'NONE',  ( -80.00000000000000000, 55.00000000000000000, 0.000000000000000000 ) ) ;
#8640 = ORIENTED_EDGE ( 'NONE', *, *, #11241, .T. ) ;
#8641 = AXIS2_PLACEMENT_3D ( 'NONE', #3583, #2802, #6353 ) ;
#8642 = AXIS2_PLACEMENT_3D ( 'NONE', #6553, #8515, #10417 ) ;
#8643 = CARTESIAN_POINT ( 'NONE',  ( -76.81250000000000000, 72.67766952966368876, -17.67766952966368876 ) ) ;
#8644 = CARTESIAN_POINT ( 'NONE',  ( -75.00000000000000000, 55.00000000000000000, 0.000000000000000000 ) ) ;
#8645 = CARTESIAN_POINT ( 'NONE',  ( -40.37827046521217511, 52.78600536084015715, -4.495190126649539764 ) ) ;
#8646 = ORIENTED_EDGE ( 'NONE', *, *, #6101, .F. ) ;
#8647 = CARTESIAN_POINT ( 'NONE',  ( -10.10988331466380430, 61.84124810089927138, -1.841955595480224250 ) ) ;
#8648 = CARTESIAN_POINT ( 'NONE',  ( -4.067038661182964928E-21, 64.99605696851786263, 19.59792961213366169 ) ) ;
#8649 = CARTESIAN_POINT ( 'NONE',  ( 3.000000000000000000, 3.673940397442059868E-16, -4.346257142857142597 ) ) ;
#8650 = CIRCLE ( 'NONE', #1172, 1.500000000000001332 ) ;
#8651 = VERTEX_POINT ( 'NONE', #10375 ) ;
#8652 = CARTESIAN_POINT ( 'NONE',  ( 16.74690967851898193, 72.97670680155702883, -12.69534381283042279 ) ) ;
#8653 = CARTESIAN_POINT ( 'NONE',  ( -75.50000000204840944, 29.18810118750000981, 10.69163855873950020 ) ) ;
#8654 = EDGE_LOOP ( 'NONE', ( #5421, #9148, #4267, #1413 ) ) ;
#8655 = CARTESIAN_POINT ( 'NONE',  ( -61.59556246352555320, 52.94114603458827872, 20.93095456750423722 ) ) ;
#8656 = B_SPLINE_CURVE_WITH_KNOTS ( 'NONE', 3,
 ( #9441, #4110, #6644, #10276, #7770, #11399, #3213, #1230, #4898, #7830, #6943, #2370, #11462, #6043, #9680, #10569, #3270, #5081, #8726, #507, #4170, #6540, #10997, #6414, #1904, #2022, #9991, #1966, #2809, #8264 ),
 .UNSPECIFIED., .F., .F.,
 ( 4, 2, 2, 2, 2, 2, 2, 2, 2, 2, 2, 2, 2, 2, 4 ),
 ( 0.04856964348838239964, 0.05008746542464584395, 0.05160528736090929519, 0.05312310929717274643, 0.05464093123343619074, 0.05615875316969964198, 0.05767657510596308629, 0.06071221897849000265, 0.06223004091475346777, 0.06374786285101693983, 0.06526568478728039802, 0.06678350672354385620, 0.06830132865980732826, 0.06981915059607078644, 0.07285479446859771668 ),
 .UNSPECIFIED. ) ;
#8657 = CARTESIAN_POINT ( 'NONE',  ( -73.53125000204839523, 36.74823131438024859, -18.25176868561973720 ) ) ;
#8658 = ADVANCED_FACE ( 'NONE', ( #4692 ), #7520, .T. ) ;
#8659 = LINE ( 'NONE', #2299, #11699 ) ;
#8660 = LINE ( 'NONE', #9489, #2407 ) ;
#8661 = CARTESIAN_POINT ( 'NONE',  ( 52.99999999999999289, 97.00000000000000000, -9.797174393178809880E-16 ) ) ;
#8662 = ORIENTED_EDGE ( 'NONE', *, *, #3591, .T. ) ;
#8663 = EDGE_CURVE ( 'NONE', #2384, #8906, #5476, .T. ) ;
#8664 = CARTESIAN_POINT ( 'NONE',  ( -80.00000000000002842, 50.75735931288069480, 5.742644059037076865 ) ) ;
#8665 = ADVANCED_FACE ( 'NONE', ( #5839 ), #10825, .T. ) ;
#8666 = CARTESIAN_POINT ( 'NONE',  ( -22.50647595179652072, 59.12487335784310005, 20.69694904210189179 ) ) ;
#8667 = ORIENTED_EDGE ( 'NONE', *, *, #9815, .T. ) ;
#8668 = CARTESIAN_POINT ( 'NONE',  ( -17.16026715680585824, 72.53745844446059721, 11.72589600754185035 ) ) ;
#8669 = CARTESIAN_POINT ( 'NONE',  ( -19.92281716047341433, 63.89755087529745481, 10.83930136440029202 ) ) ;
#8670 = CARTESIAN_POINT ( 'NONE',  ( 37.00000000000000000, 55.00000000000000000, 0.000000000000000000 ) ) ;
#8671 = DIRECTION ( 'NONE',  ( 1.000000000000000000, 6.033820786006286457E-17, -0.000000000000000000 ) ) ;
#8672 = DIRECTION ( 'NONE',  ( -1.000000000000000000, 0.000000000000000000, 0.000000000000000000 ) ) ;
#8673 = VERTEX_POINT ( 'NONE', #6683 ) ;
#8674 = CARTESIAN_POINT ( 'NONE',  ( -73.34375000000001421, 65.35533905932737753, 24.99999999999999645 ) ) ;
#8675 = CARTESIAN_POINT ( 'NONE',  ( -68.34104732181945963, 33.99448141944315438, 0.006743540747239065887 ) ) ;
#8676 = CARTESIAN_POINT ( 'NONE',  ( -15.00000000000000355, 5.000000000000000000, 30.00000000000000711 ) ) ;
#8677 = FACE_OUTER_BOUND ( 'NONE', #6092, .T. ) ;
#8678 = CARTESIAN_POINT ( 'NONE',  ( -43.87484156505298216, 56.02863006267562440, -6.935366095584925006 ) ) ;
#8679 = VERTEX_POINT ( 'NONE', #1027 ) ;
#8680 = CARTESIAN_POINT ( 'NONE',  ( -17.88142570751413274, 67.52739394234649239, 16.89079266652326439 ) ) ;
#8681 = CARTESIAN_POINT ( 'NONE',  ( 23.00000000000000000, 76.00000000000000000, 0.000000000000000000 ) ) ;
#8682 = DIRECTION ( 'NONE',  ( 0.000000000000000000, 0.000000000000000000, -1.000000000000000000 ) ) ;
#8683 = CARTESIAN_POINT ( 'NONE',  ( -77.75000000204839523, 65.69163855873948421, -25.81189881250000084 ) ) ;
#8684 = EDGE_CURVE ( 'NONE', #9755, #11556, #9480, .T. ) ;
#8685 = CARTESIAN_POINT ( 'NONE',  ( -19.49409276286124637, 75.18365745446243409, 14.82016776532273816 ) ) ;
#8686 = CARTESIAN_POINT ( 'NONE',  ( -73.90625000204839523, 36.74823131438026280, 18.25176868561974786 ) ) ;
#8687 = VERTEX_POINT ( 'NONE', #7633 ) ;
#8688 = CARTESIAN_POINT ( 'NONE',  ( -76.43750000409679046, 37.32233047033631124, 17.67766952966369232 ) ) ;
#8689 = FACE_BOUND ( 'NONE', #8456, .T. ) ;
#8690 = FACE_BOUND ( 'NONE', #10556, .T. ) ;
#8691 = CARTESIAN_POINT ( 'NONE',  ( -28.36397722366938012, 36.00052710555507218, 8.986026874162561739 ) ) ;
#8692 = CARTESIAN_POINT ( 'NONE',  ( -75.31250000000005684, 72.67766952966361771, -17.67766952966360705 ) ) ;
#8693 = AXIS2_PLACEMENT_3D ( 'NONE', #11657, #10698, #5266 ) ;
#8694 = DIRECTION ( 'NONE',  ( 1.000000000000000000, 6.033820786006286457E-17, 0.000000000000000000 ) ) ;
#8695 = DIRECTION ( 'NONE',  ( -0.000000000000000000, -0.000000000000000000, -1.000000000000000000 ) ) ;
#8696 = ORIENTED_EDGE ( 'NONE', *, *, #5711, .F. ) ;
#8697 = DIRECTION ( 'NONE',  ( 0.000000000000000000, 1.000000000000000000, 0.000000000000000000 ) ) ;
#8698 = CARTESIAN_POINT ( 'NONE',  ( -72.31250000000000000, 72.67766952966368876, -17.67766952966368876 ) ) ;
#8699 = DIRECTION ( 'NONE',  ( 0.000000000000000000, 1.000000000000000000, 0.000000000000000000 ) ) ;
#8700 = ADVANCED_FACE ( 'NONE', ( #1988 ), #9358, .F. ) ;
#8701 = CARTESIAN_POINT ( 'NONE',  ( -44.07273810123712110, 55.81934495312422939, -4.935102682546041564 ) ) ;
#8702 = ORIENTED_EDGE ( 'NONE', *, *, #4324, .T. ) ;
#8703 = CARTESIAN_POINT ( 'NONE',  ( -42.29128031504409080, 58.00020108910005234, -6.342998449018511842 ) ) ;
#8704 = CARTESIAN_POINT ( 'NONE',  ( 0.000000000000000000, 0.000000000000000000, -6.099999999999997868 ) ) ;
#8705 = EDGE_CURVE ( 'NONE', #8766, #8631, #1269, .T. ) ;
#8706 = LINE ( 'NONE', #8649, #7406 ) ;
#8707 = ORIENTED_EDGE ( 'NONE', *, *, #8663, .F. ) ;
#8708 = CARTESIAN_POINT ( 'NONE',  ( 20.32841434030235561, 75.84512567670806504, 7.042511973064372377 ) ) ;
#8709 = DIRECTION ( 'NONE',  ( -0.000000000000000000, -0.000000000000000000, -1.000000000000000000 ) ) ;
#8710 = ORIENTED_EDGE ( 'NONE', *, *, #4053, .F. ) ;
#8711 = CARTESIAN_POINT ( 'NONE',  ( -73.62500000204842365, 29.18810118750000626, -10.69163855873949309 ) ) ;
#8712 = ADVANCED_FACE ( 'NONE', ( #8341 ), #9419, .T. ) ;
#8713 = CARTESIAN_POINT ( 'NONE',  ( -75.59375000409677625, 80.00000000000001421, -10.35533905932737753 ) ) ;
#8714 = CARTESIAN_POINT ( 'NONE',  ( -8.430468385592622127, 54.98139370647056978, 0.006371973333601899971 ) ) ;
#8715 = LINE ( 'NONE', #2301, #5481 ) ;
#8716 = VERTEX_POINT ( 'NONE', #5657 ) ;
#8717 = LINE ( 'NONE', #9670, #2432 ) ;
#8718 = CARTESIAN_POINT ( 'NONE',  ( -32.11869219899978845, 34.20636958863568822, 3.085052597841025701 ) ) ;
#8719 = ORIENTED_EDGE ( 'NONE', *, *, #7570, .T. ) ;
#8720 = CARTESIAN_POINT ( 'NONE',  ( -8.118692201255964136, 67.52163282122538135, -16.88455524069670233 ) ) ;
#8721 = CARTESIAN_POINT ( 'NONE',  ( -38.79377121134427142, 46.38247438902519093, -11.20693327228071468 ) ) ;
#8722 = DIRECTION ( 'NONE',  ( 0.000000000000000000, 1.000000000000000000, 0.000000000000000000 ) ) ;
#8723 = CARTESIAN_POINT ( 'NONE',  ( -76.34375000409679046, 30.00000000000001421, 10.35533905932739174 ) ) ;
#8724 = B_SPLINE_SURFACE_WITH_KNOTS ( 'NONE', 3, 3, ( 
 ( #11174, #8380, #5695, #3945, #7369, #5569, #2808, #4607, #6598, #8316, #226, #6655, #9216, #10289, #161, #3831, #3889, #1004, #2869, #2083, #7496, #10103, #6536, #5757, #7609, #10168, #2020, #9269, #9394, #38, #9332, #4788, #1188, #4853, #8502, #1122, #4663, #3048, #1901, #6718, #10350, #5510, #941, #11531, #4070, #10460, #6835, #5145, #1240, #5034, #9631, #8562, #8680, #5933, #3281, #11412, #4972, #10518, #2325, #6778, #2147, #11302, #10405, #2378, #405, #1426, #342, #9574, #1371, #10577, #463, #8798, #7727, #6951, #5997, #11358, #4910, #576, #3112, #2261, #4120, #6053, #7667, #9688, #9455, #4008, #5817, #2205, #1486, #5872, #4243, #7902, #3337, #7780, #5089, #7007, #3165, #3222, #6891, #8736, #8623, #9514, #1304, #519, #4181, #7842, #11470, #1540, #1652, #9918, #7246, #3575, #1771, #8082, #10696, #692, #636, #11715, #2618, #6171, #2681, #8190, #4365, #7130 ),
 ( #4534, #11655, #11826, #4298, #863, #4424, #2444, #3515, #3633, #6110, #10809, #809, #6228, #4478, #7184, #5207, #10868, #9743, #9802, #6345, #5437, #750, #10629, #8857, #1716, #7957, #11591, #9976, #6287, #5380, #3397, #9084, #8130, #3464, #7070, #2506, #2561, #9032, #1596, #11768, #5264, #8911, #8016, #10752, #9859, #5321, #8974, #5677, #6400, #10148, #11158, #1106, #2741, #1949, #7414, #2973, #2917, #5618, #8489, #84, #8363, #7356, #9198, #2793, #10212, #10030, #1884, #3692, #10271, #3747, #1823, #6639, #2069, #8247, #8426, #145, #5492, #9317, #9257, #7481, #5740, #9142, #10981, #923, #4591, #1047, #10087, #2005, #4770, #6457, #989, #24, #4712, #11102, #5555, #9376, #4837, #4650, #11042, #2850, #1169, #8303, #3811, #6582, #6520, #210, #3875, #7536, #267, #7301, #10931, #449, #8545, #3930, #1226, #327, #4165, #2187, #11395, #10333, #7714, #11343, #503, #3151 ),
 ( #5859, #6702, #2367, #4893, #8611, #389, #7826, #9437, #5077, #11223, #2130, #7594, #3992, #11458, #5803, #7652, #1414, #11285, #3098, #9498, #10504, #3267, #2308, #5021, #6938, #1354, #10566, #9560, #1288, #6764, #10391, #4955, #5985, #6039, #3033, #9675, #1471, #8720, #4058, #6819, #5134, #4106, #10445, #9619, #7764, #8782, #2247, #5916, #8668, #3209, #6877, #3326, #2491, #7234, #5192, #1703, #8899, #8963, #10796, #679, #10617, #6155, #6994, #2428, #4352, #10859, #3562, #11756, #8003, #737, #9963, #9791, #11638, #3444, #4412, #3381, #9019, #2667, #7058, #6214, #10678, #7172, #6096, #7116, #11705, #795, #5367, #6334, #9847, #623, #9728, #4287, #1528, #11520, #1639, #1584, #3505, #6276, #7945, #9907, #10741, #2548, #2607, #11579, #5252, #4469, #5308, #8063, #8121, #1759, #5424, #563, #4230, #7889, #8844, #1034, #70, #7467, #3621, #3734, #194, #10073, #8412, #7400 ),
 ( #1095, #6628, #10970, #5539, #1872, #3863, #8177, #11028, #4697, #7288, #2837, #975, #10200, #6505, #12, #5607, #9246, #1811, #9074, #6388, #5479, #9301, #7345, #8348, #10919, #4640, #8292, #5664, #10133, #7525, #2781, #1994, #132, #6443, #11816, #11147, #10016, #9186, #1935, #4759, #2731, #2962, #4522, #9128, #850, #909, #10258, #4580, #8235, #6572, #3682, #3797, #11090, #2903, #2055, #4260, #6805, #1559, #3139, #9760, #11331, #11270, #3021, #2115, #9425, #7918, #5225, #5729, #6126, #652, #10648, #6688, #7640, #3352, #2235, #7583, #11549, #5904, #2459, #9485, #8873, #3981, #1154, #435, #8477, #3081, #4317, #10319, #7025, #7973, #11610, #10433, #5792, #6752, #11210, #9548, #1343, #1215, #3413, #7087, #10380, #2175, #5844, #10711, #4824, #8600, #5006, #253, #376, #1275, #9363, #8655, #8532, #3918, #4881, #316, #4943, #4041, #7698, #2756, #767, #9992, #8930, #6304 ) ),
 .UNSPECIFIED., .F., .F., .F.,
 ( 4, 4 ),
 ( 4, 2, 2, 2, 2, 2, 2, 2, 2, 2, 2, 2, 2, 2, 2, 2, 2, 2, 2, 2, 2, 2, 2, 2, 2, 2, 2, 2, 2, 2, 2, 2, 2, 2, 2, 2, 2, 2, 2, 2, 2, 2, 2, 2, 2, 2, 2, 2, 2, 2, 2, 2, 2, 2, 2, 2, 2, 2, 2, 2, 2, 4 ),
 ( 0.000000000000000000, 1.000000000000000000 ),
 ( 0.000000000000000000, 0.02499977550252127645, 0.04999988577693819519, 0.07499999605135511394, 0.09999999831535408279, 0.1250000005793530378, 0.1500000028441162425, 0.1750000051088794195, 0.1937500039558066045, 0.2031250033792701970, 0.2125000028027338173, 0.2218750022261974375, 0.2312500016496610300, 0.2500000004965882150, 0.2750000027613288545, 0.3000000050260694384, 0.3187500038730080032, 0.3281250032964772578, 0.3375000027199465125, 0.3468750021434158226, 0.3562500015668850772, 0.3750000004138236420, 0.4000000026785641705, 0.4250000049433046989, 0.4437500037902432082, 0.4531250032137125183, 0.4625000026371817730, 0.4718750020606510276, 0.4812500014841203377, 0.5000000003310588470, 0.5250000025957997085, 0.5500000048605405700, 0.5687500037074788573, 0.5781250031309480564, 0.5875000025544172555, 0.5968750019778864546, 0.6062500014013556537, 0.6250000002482940520, 0.6500000025128280789, 0.6750000047773621059, 0.6937500036244039769, 0.7031250030479249125, 0.7125000024714458480, 0.7218750018949667835, 0.7312500013184877190, 0.7500000001655295900, 0.7750000023794885173, 0.8000000045934475557, 0.8187500034657768655, 0.8281250029019414649, 0.8375000023381060643, 0.8468750017742707747, 0.8562500012104353742, 0.8750000000827646840, 0.8937502654913498379, 0.9031253981956424148, 0.9125005308999349918, 0.9218756636042275687, 0.9312507963085201457, 0.9500010617171052996, 0.9750005308585526498, 1.000000000000000000 ),
 .UNSPECIFIED. ) ;
#8725 = VECTOR ( 'NONE', #9506, 1000.000000000000000 ) ;
#8726 = CARTESIAN_POINT ( 'NONE',  ( -26.37503197251934850, 53.38964644461982090, 4.744911376643659473 ) ) ;
#8727 = EDGE_LOOP ( 'NONE', ( #6108, #10147, #4206, #6544 ) ) ;
#8728 = CARTESIAN_POINT ( 'NONE',  ( -78.68750000204838102, 44.30836144126053000, 25.81189881250000795 ) ) ;
#8729 = CARTESIAN_POINT ( 'NONE',  ( -74.99999999999997158, 47.61856851181366324, -24.74822985635785599 ) ) ;
#8730 = CARTESIAN_POINT ( 'NONE',  ( -78.00000000000001421, 50.75735931288069480, -12.72791868944003824 ) ) ;
#8731 = CONICAL_SURFACE ( 'NONE', #6445, 5.000000000000000888, 1.047197551196596299 ) ;
#8732 = DIRECTION ( 'NONE',  ( -1.000000000000000000, -0.000000000000000000, -0.000000000000000000 ) ) ;
#8733 = CARTESIAN_POINT ( 'NONE',  ( -20.54150823158944661, 59.17669310859397314, 5.631395700702261919 ) ) ;
#8734 = ORIENTED_EDGE ( 'NONE', *, *, #1684, .T. ) ;
#8735 = EDGE_CURVE ( 'NONE', #10918, #8848, #7021, .T. ) ;
#8736 = CARTESIAN_POINT ( 'NONE',  ( -52.59603425219209782, 73.55155261293346314, 9.913157997185967574 ) ) ;
#8737 = CIRCLE ( 'NONE', #10254, 1.500000000000001332 ) ;
#8738 = CYLINDRICAL_SURFACE ( 'NONE', #490, 1.499999999999999556 ) ;
#8739 = CARTESIAN_POINT ( 'NONE',  ( -5.000000000000000000, 2.886751345948126879, -6.099999999999999645 ) ) ;
#8740 = CARTESIAN_POINT ( 'NONE',  ( -74.28125000204839523, 73.25176868561975141, 18.25176868561974075 ) ) ;
#8741 = CARTESIAN_POINT ( 'NONE',  ( -24.47794101355583862, 79.30561927337025452, -5.910399932586783756 ) ) ;
#8742 = CARTESIAN_POINT ( 'NONE',  ( -74.37500000204838102, 80.81189881250001861, 10.69163855873948599 ) ) ;
#8743 = VERTEX_POINT ( 'NONE', #1147 ) ;
#8744 = CARTESIAN_POINT ( 'NONE',  ( -74.93750000409677625, 37.32233047033631124, 17.67766952966369232 ) ) ;
#8745 = CARTESIAN_POINT ( 'NONE',  ( -3.000000000000000888, 3.673940397442060854E-16, -25.03750572909317285 ) ) ;
#8746 = CARTESIAN_POINT ( 'NONE',  ( -75.96875000000005684, 30.00000000000011013, 10.35533905932735088 ) ) ;
#8747 = CARTESIAN_POINT ( 'NONE',  ( 9.477680475861957277, 36.67126955513442255, 10.56417786655960356 ) ) ;
#8748 = VECTOR ( 'NONE', #11622, 1000.000000000000000 ) ;
#8749 = CARTESIAN_POINT ( 'NONE',  ( -75.12500000000007105, 79.99999999999988631, -1.530808498934184619E-15 ) ) ;
#8750 = AXIS2_PLACEMENT_3D ( 'NONE', #4888, #6151, #7822 ) ;
#8751 = LINE ( 'NONE', #533, #2039 ) ;
#8752 = DIRECTION ( 'NONE',  ( 0.000000000000000000, 0.000000000000000000, 1.000000000000000000 ) ) ;
#8753 = ORIENTED_EDGE ( 'NONE', *, *, #11425, .F. ) ;
#8754 = DIRECTION ( 'NONE',  ( -1.000000000000000000, 0.000000000000000000, 0.000000000000000000 ) ) ;
#8755 = AXIS2_PLACEMENT_3D ( 'NONE', #8261, #1118, #36 ) ;
#8756 = CARTESIAN_POINT ( 'NONE',  ( -76.71875000000000000, 80.00000000000001421, -10.35533905932737753 ) ) ;
#8757 = DIRECTION ( 'NONE',  ( 0.000000000000000000, 1.000000000000000000, 0.000000000000000000 ) ) ;
#8758 = COLOUR_RGB ( '',0.8941176470588234615, 0.8941176470588234615, 0.8941176470588234615 ) ;
#8759 = DIRECTION ( 'NONE',  ( 0.000000000000000000, 0.000000000000000000, -1.000000000000000000 ) ) ;
#8760 = ORIENTED_EDGE ( 'NONE', *, *, #2416, .T. ) ;
#8761 =( BOUNDED_CURVE ( )  B_SPLINE_CURVE ( 2, ( #1893, #8255, #7425, #5388, #8198, #6406, #11774 ),
 .UNSPECIFIED., .F., .T. ) 
 B_SPLINE_CURVE_WITH_KNOTS ( ( 3, 2, 2, 3 ),
 ( 0.8333333333333340365, 0.8541666666666670737, 0.8750000000000002220, 0.8888490476107191451 ),
 .UNSPECIFIED. ) 
 CURVE ( )  GEOMETRIC_REPRESENTATION_ITEM ( )  RATIONAL_B_SPLINE_CURVE ( ( 0.9999999999999975575, 0.9238795325112891810, 1.000000000000000000, 0.9238795325112867385, 1.000000000000000000, 0.9493985930367334625, 0.9660721903170175207 ) ) 
 REPRESENTATION_ITEM ( '' )  );
#8762 = CARTESIAN_POINT ( 'NONE',  ( -53.66679727893465923, 59.95398294780274995, 4.953507936222676378 ) ) ;
#8763 = CARTESIAN_POINT ( 'NONE',  ( -83.00000000000000000, 55.00000000000000000, 0.000000000000000000 ) ) ;
#8764 = FACE_OUTER_BOUND ( 'NONE', #4642, .T. ) ;
#8765 = CIRCLE ( 'NONE', #720, 24.99999999999999645 ) ;
#8766 = VERTEX_POINT ( 'NONE', #11020 ) ;
#8767 = CARTESIAN_POINT ( 'NONE',  ( 3.623988215512224720, 65.45978901809303352, -19.35591671848164097 ) ) ;
#8768 = DIRECTION ( 'NONE',  ( 0.000000000000000000, 1.000000000000000000, 0.000000000000000000 ) ) ;
#8769 = VERTEX_POINT ( 'NONE', #6498 ) ;
#8770 = CARTESIAN_POINT ( 'NONE',  ( -79.06250000204840944, 80.81189881250001861, -10.69163855873949132 ) ) ;
#8771 = EDGE_CURVE ( 'NONE', #9843, #4769, #10128, .T. ) ;
#8772 = LINE ( 'NONE', #8552, #10337 ) ;
#8773 = EDGE_CURVE ( 'NONE', #7395, #8040, #7220, .T. ) ;
#8774 = LINE ( 'NONE', #3319, #5589 ) ;
#8775 = CARTESIAN_POINT ( 'NONE',  ( -4.909738907900197624, 55.00455243144571682, -0.008585322715572331689 ) ) ;
#8776 = CARTESIAN_POINT ( 'NONE',  ( -75.00000000000000000, 31.79283308196307445, 9.999956478894377554 ) ) ;
#8777 = ORIENTED_EDGE ( 'NONE', *, *, #8281, .T. ) ;
#8778 = CARTESIAN_POINT ( 'NONE',  ( -15.00000000000000000, 5.000000000000000000, -20.00000000000000000 ) ) ;
#8779 = EDGE_CURVE ( 'NONE', #6614, #10565, #8737, .T. ) ;
#8780 = CARTESIAN_POINT ( 'NONE',  ( -48.52239103406665066, 73.33336493528216238, -10.56581381373428208 ) ) ;
#8781 = ORIENTED_EDGE ( 'NONE', *, *, #4863, .T. ) ;
#8782 = CARTESIAN_POINT ( 'NONE',  ( -14.47762819197135364, 76.02046563874422702, 2.745652569741364957 ) ) ;
#8783 = CARTESIAN_POINT ( 'NONE',  ( -22.83648567187163181, 57.75017295826287977, 13.79876555885540590 ) ) ;
#8784 = CARTESIAN_POINT ( 'NONE',  ( -74.28125000204838102, 55.00000000000000000, 25.81189881249999729 ) ) ;
#8785 = CIRCLE ( 'NONE', #4961, 1.500000000000001332 ) ;
#8786 = ORIENTED_EDGE ( 'NONE', *, *, #931, .T. ) ;
#8787 = CARTESIAN_POINT ( 'NONE',  ( -73.62500000000000000, 80.00000000000000000, -1.530808498934191324E-15 ) ) ;
#8788 = DIRECTION ( 'NONE',  ( 0.000000000000000000, 1.000000000000000000, 0.000000000000000000 ) ) ;
#8789 = B_SPLINE_CURVE_WITH_KNOTS ( 'NONE', 3,
 ( #7708, #10388, #2243, #608, #4054, #11340, #7039, #8608 ),
 .UNSPECIFIED., .F., .F.,
 ( 4, 2, 2, 4 ),
 ( 0.002921158011986710757, 0.003648658599403065313, 0.004376159186819420302, 0.005831160361652131148 ),
 .UNSPECIFIED. ) ;
#8790 = VERTEX_POINT ( 'NONE', #9240 ) ;
#8791 = DIRECTION ( 'NONE',  ( -1.000000000000000000, -0.000000000000000000, -0.000000000000000000 ) ) ;
#8792 = EDGE_CURVE ( 'NONE', #1955, #8561, #1766, .T. ) ;
#8793 = AXIS2_PLACEMENT_3D ( 'NONE', #7960, #8802, #8914 ) ;
#8794 = CARTESIAN_POINT ( 'NONE',  ( 9.042618572576390790, 50.25505735147245190, 1.610274559975814812 ) ) ;
#8795 = CARTESIAN_POINT ( 'NONE',  ( -31.33319364550761321, 48.52303905584467003, 2.682555320553783762 ) ) ;
#8796 = AXIS2_PLACEMENT_3D ( 'NONE', #8024, #6295, #7253 ) ;
#8797 = ORIENTED_EDGE ( 'NONE', *, *, #2342, .F. ) ;
#8798 = CARTESIAN_POINT ( 'NONE',  ( -30.99614452189004155, 33.97742542711323921, 0.0005215828242728561687 ) ) ;
#8799 = CARTESIAN_POINT ( 'NONE',  ( 0.000000000000000000, 0.000000000000000000, -3.131981945180866589 ) ) ;
#8800 = DIRECTION ( 'NONE',  ( -0.000000000000000000, -0.000000000000000000, -1.000000000000000000 ) ) ;
#8801 = CARTESIAN_POINT ( 'NONE',  ( -77.65625000204839523, 73.25176868561975141, -18.25176868561974430 ) ) ;
#8802 = DIRECTION ( 'NONE',  ( 0.000000000000000000, 1.000000000000000000, 0.000000000000000000 ) ) ;
#8803 = CARTESIAN_POINT ( 'NONE',  ( -72.87500000204840944, 80.81189881250001861, 10.69163855873948599 ) ) ;
#8804 = EDGE_CURVE ( 'NONE', #5658, #3322, #9296, .T. ) ;
#8805 = EDGE_CURVE ( 'NONE', #9206, #9472, #7871, .T. ) ;
#8806 = ORIENTED_EDGE ( 'NONE', *, *, #6552, .T. ) ;
#8807 = CARTESIAN_POINT ( 'NONE',  ( -75.31250000409677625, 72.67766952966368876, 17.67766952966368521 ) ) ;
#8808 = FACE_OUTER_BOUND ( 'NONE', #3289, .T. ) ;
#8809 = CARTESIAN_POINT ( 'NONE',  ( -75.00000000000001421, 58.46699551781524917, -25.57799957749213604 ) ) ;
#8810 = VECTOR ( 'NONE', #6098, 1000.000000000000000 ) ;
#8811 = CARTESIAN_POINT ( 'NONE',  ( -9.391823749396904120, 73.59702374900430755, -9.931971109272440756 ) ) ;
#8812 = FACE_OUTER_BOUND ( 'NONE', #3417, .T. ) ;
#8813 = EDGE_CURVE ( 'NONE', #3881, #3861, #11781, .T. ) ;
#8814 = DIRECTION ( 'NONE',  ( 0.000000000000000000, 0.000000000000000000, 1.000000000000000000 ) ) ;
#8815 = VECTOR ( 'NONE', #8961, 1000.000000000000000 ) ;
#8816 = CARTESIAN_POINT ( 'NONE',  ( 2.925285743277525441, 4.084588180558403003, -6.089444439476610071 ) ) ;
#8817 = CARTESIAN_POINT ( 'NONE',  ( -78.12500000204838102, 44.30836144126050158, -25.81189881249999374 ) ) ;
#8818 = CARTESIAN_POINT ( 'NONE',  ( -80.00000000000001421, 50.75735931288069480, -4.242637315201482906 ) ) ;
#8819 = ORIENTED_EDGE ( 'NONE', *, *, #5073, .F. ) ;
#8820 = CYLINDRICAL_SURFACE ( 'NONE', #8829, 5.249999999999998224 ) ;
#8821 = AXIS2_PLACEMENT_3D ( 'NONE', #6494, #6432, #8280 ) ;
#8822 = PRODUCT_DEFINITION_CONTEXT ( 'detailed design', #11501, 'design' ) ;
#8823 = ORIENTED_EDGE ( 'NONE', *, *, #2725, .T. ) ;
#8824 = CARTESIAN_POINT ( 'NONE',  ( -67.66638273083707134, 47.99409686189664370, 0.0004508834932907918535 ) ) ;
#8825 = CIRCLE ( 'NONE', #10720, 3.000000000000000000 ) ;
#8826 = CARTESIAN_POINT ( 'NONE',  ( 0.000000000000000000, 110.0000000000000000, 0.000000000000000000 ) ) ;
#8827 = CARTESIAN_POINT ( 'NONE',  ( -78.87500000409677625, 55.00000000000000000, -24.99999999999999645 ) ) ;
#8828 = CARTESIAN_POINT ( 'NONE',  ( 21.49960740303508544, 76.81950186437471473, -2.905261289213686204 ) ) ;
#8829 = AXIS2_PLACEMENT_3D ( 'NONE', #2401, #8101, #1447 ) ;
#8830 = VECTOR ( 'NONE', #11132, 1000.000000000000000 ) ;
#8831 = CARTESIAN_POINT ( 'NONE',  ( -72.59375000204838102, 36.74823131438026280, 18.25176868561974786 ) ) ;
#8832 = ORIENTED_EDGE ( 'NONE', *, *, #11645, .T. ) ;
#8833 = CARTESIAN_POINT ( 'NONE',  ( -76.34375000204839523, 55.00000000000000000, -25.81189881249999729 ) ) ;
#8834 = CARTESIAN_POINT ( 'NONE',  ( -79.25000000000000000, 55.00000000000000000, 24.99999999999999645 ) ) ;
#8835 = CARTESIAN_POINT ( 'NONE',  ( 3.000000000000000000, 3.673940397442059868E-16, -3.482085714285714229 ) ) ;
#8836 = CARTESIAN_POINT ( 'NONE',  ( 24.42601517758169294, 54.97644996077841739, -0.01153606584382102333 ) ) ;
#8837 = CARTESIAN_POINT ( 'NONE',  ( 59.09999999999999432, 55.00000000000001421, -3.686287386450715076E-15 ) ) ;
#8838 = CIRCLE ( 'NONE', #687, 1.500000000000001332 ) ;
#8839 = DIRECTION ( 'NONE',  ( 1.000000000000000000, 0.000000000000000000, 0.000000000000000000 ) ) ;
#8840 = EDGE_LOOP ( 'NONE', ( #3944, #10904 ) ) ;
#8841 = CARTESIAN_POINT ( 'NONE',  ( -29.84797894700232490, 49.99999999999998579, 0.3308608129958152677 ) ) ;
#8842 = CARTESIAN_POINT ( 'NONE',  ( -30.67054324275970600, 35.57292846186890500, 8.046485333435041909 ) ) ;
#8843 = ORIENTED_EDGE ( 'NONE', *, *, #8439, .F. ) ;
#8844 = CARTESIAN_POINT ( 'NONE',  ( -62.06863883070810317, 48.89596633111685975, 20.11004999522056025 ) ) ;
#8845 = CARTESIAN_POINT ( 'NONE',  ( -27.87283258141598097, 46.40806184526439893, 11.18159849702474240 ) ) ;
#8846 = CONICAL_SURFACE ( 'NONE', #577, 5.000000000000000888, 1.047197551196596299 ) ;
#8847 = CARTESIAN_POINT ( 'NONE',  ( -78.78125000204838102, 55.00000000000000000, 25.81189881249999729 ) ) ;
#8848 = VERTEX_POINT ( 'NONE', #6863 ) ;
#8849 = CARTESIAN_POINT ( 'NONE',  ( -74.56250000000000000, 37.32233047033631124, 17.67766952966369232 ) ) ;
#8850 = DIRECTION ( 'NONE',  ( 0.000000000000000000, 1.000000000000000000, 0.000000000000000000 ) ) ;
#8851 = VERTEX_POINT ( 'NONE', #5173 ) ;
#8852 = SURFACE_STYLE_USAGE ( .BOTH. , #11405 ) ;
#8853 = ADVANCED_FACE ( 'NONE', ( #8764 ), #11326, .F. ) ;
#8854 = FACE_OUTER_BOUND ( 'NONE', #8028, .T. ) ;
#8855 = CARTESIAN_POINT ( 'NONE',  ( -13.44321664086546875, 61.83368541783048755, -1.838823801362371668 ) ) ;
#8856 = ORIENTED_EDGE ( 'NONE', *, *, #447, .F. ) ;
#8857 = CARTESIAN_POINT ( 'NONE',  ( 3.337188803346179178, 35.57729950087108506, -8.044583786737664610 ) ) ;
#8858 = MANIFOLD_SOLID_BREP ( 'AdvancedHole1', #1942 ) ;
#8859 = LINE ( 'NONE', #4366, #2602 ) ;
#8860 = CARTESIAN_POINT ( 'NONE',  ( -78.00000000000001421, 63.48528137423857487, -8.485278002320759683 ) ) ;
#8861 = DIRECTION ( 'NONE',  ( -0.8191520442889974607, 0.000000000000000000, -0.5735764363510379438 ) ) ;
#8862 = CARTESIAN_POINT ( 'NONE',  ( -73.06250000204840944, 80.81189881250001861, -10.69163855873949132 ) ) ;
#8863 = ORIENTED_EDGE ( 'NONE', *, *, #9812, .F. ) ;
#8864 = CARTESIAN_POINT ( 'NONE',  ( -71.56250000409677625, 37.32233047033631124, -17.67766952966368166 ) ) ;
#8865 = CARTESIAN_POINT ( 'NONE',  ( -78.00000000000001421, 67.72792206135787296, -12.72791868944004534 ) ) ;
#8866 = CARTESIAN_POINT ( 'NONE',  ( -67.17811141605125158, 49.99997012509656713, 0.3311688885648463310 ) ) ;
#8867 = CARTESIAN_POINT ( 'NONE',  ( -17.88142570751413274, 67.52739394234649239, 16.89079266652326439 ) ) ;
#8868 = ORIENTED_EDGE ( 'NONE', *, *, #6760, .F. ) ;
#8869 = CARTESIAN_POINT ( 'NONE',  ( -75.78125000204838102, 55.00000000000000000, 25.81189881249999729 ) ) ;
#8870 = CARTESIAN_POINT ( 'NONE',  ( -66.81138001472987753, 51.23444936853855580, 3.305681383735873613 ) ) ;
#8871 = ADVANCED_FACE ( 'NONE', ( #6080 ), #609, .F. ) ;
#8872 = LINE ( 'NONE', #5451, #4752 ) ;
#8873 = CARTESIAN_POINT ( 'NONE',  ( -41.16026710375170694, 50.89060761561553647, -20.69263693287480521 ) ) ;
#8874 = CARTESIAN_POINT ( 'NONE',  ( 0.000000000000000000, -57.00000000000000000, 0.000000000000000000 ) ) ;
#8875 = CARTESIAN_POINT ( 'NONE',  ( -75.12500000204838102, 44.30836144126050158, -25.81189881249999374 ) ) ;
#8876 = CARTESIAN_POINT ( 'NONE',  ( 47.00000000000000000, 51.46446609406726935, 3.535533905932731091 ) ) ;
#8877 = ORIENTED_EDGE ( 'NONE', *, *, #9211, .F. ) ;
#8878 = DIRECTION ( 'NONE',  ( 1.000000000000000000, 0.000000000000000000, 0.000000000000000000 ) ) ;
#8879 = EDGE_LOOP ( 'NONE', ( #2840, #9618, #6084, #6763 ) ) ;
#8880 = EDGE_CURVE ( 'NONE', #5516, #9669, #10055, .T. ) ;
#8881 = CARTESIAN_POINT ( 'NONE',  ( -43.75092013918801115, 59.45036911068460483, -5.422234973716651751 ) ) ;
#8882 = FACE_BOUND ( 'NONE', #3531, .T. ) ;
#8883 = LINE ( 'NONE', #662, #8748 ) ;
#8884 = CARTESIAN_POINT ( 'NONE',  ( 21.67169741744320888, 76.96394498674538909, -1.454759563390118471 ) ) ;
#8885 = CARTESIAN_POINT ( 'NONE',  ( 5.000000000000000000, 2.419979747126329350, -5.788163366729714099 ) ) ;
#8886 = VERTEX_POINT ( 'NONE', #1336 ) ;
#8887 = ADVANCED_FACE ( 'NONE', ( #6021 ), #2411, .F. ) ;
#8888 = CARTESIAN_POINT ( 'NONE',  ( -76.90625000204839523, 36.74823131438026280, 18.25176868561974786 ) ) ;
#8889 = DIRECTION ( 'NONE',  ( 0.000000000000000000, 1.000000000000000000, 0.000000000000000000 ) ) ;
#8890 = CARTESIAN_POINT ( 'NONE',  ( 34.00000000000000000, 59.99999999999998579, 0.000000000000000000 ) ) ;
#8891 = CARTESIAN_POINT ( 'NONE',  ( 25.24065896695082145, 55.02620812721863786, 0.001656341455649923368 ) ) ;
#8892 = DIRECTION ( 'NONE',  ( 1.000000000000000000, 0.000000000000000000, 0.000000000000000000 ) ) ;
#8893 = CARTESIAN_POINT ( 'NONE',  ( -75.00000000000000000, 30.98212383677083892, -8.811831842167247686 ) ) ;
#8894 = ORIENTED_EDGE ( 'NONE', *, *, #2655, .F. ) ;
#8895 = DIRECTION ( 'NONE',  ( 9.813077866773612233E-16, -1.000000000000000000, -0.000000000000000000 ) ) ;
#8896 = EDGE_CURVE ( 'NONE', #11337, #1706, #3946, .T. ) ;
#8897 = CARTESIAN_POINT ( 'NONE',  ( -61.59556246352555320, 52.94114603458827872, 20.93095456750423722 ) ) ;
#8898 = ORIENTED_EDGE ( 'NONE', *, *, #10409, .F. ) ;
#8899 = CARTESIAN_POINT ( 'NONE',  ( -20.96936038908104649, 62.08580392802151948, 19.80242024469750817 ) ) ;
#8900 = CARTESIAN_POINT ( 'NONE',  ( -54.03632049363248768, 68.19182434251506209, 4.719955684811743879 ) ) ;
#8901 = CARTESIAN_POINT ( 'NONE',  ( -79.15625000204838102, 80.81189881250000440, -1.580522963032174394E-15 ) ) ;
#8902 = ORIENTED_EDGE ( 'NONE', *, *, #10323, .T. ) ;
#8903 = CARTESIAN_POINT ( 'NONE',  ( -72.68750000000000000, 37.32233047033631124, -17.67766952966368166 ) ) ;
#8904 = CARTESIAN_POINT ( 'NONE',  ( 12.52240408941406535, 44.41801188983610871, 18.37272825892985040 ) ) ;
#8905 = PRESENTATION_STYLE_ASSIGNMENT (( #5044 ) ) ;
#8906 = VERTEX_POINT ( 'NONE', #11381 ) ;
#8907 = CARTESIAN_POINT ( 'NONE',  ( -78.00000000000001421, 59.24264068711927678, 5.742644059037073312 ) ) ;
#8908 = CARTESIAN_POINT ( 'NONE',  ( -70.87427368927673399, 76.65063840437989029, 12.49999426731031704 ) ) ;
#8909 = CARTESIAN_POINT ( 'NONE',  ( 8.759403238133714353, 55.01273213413052332, -0.01040348312344842492 ) ) ;
#8910 = EDGE_LOOP ( 'NONE', ( #5076, #6279, #8397, #6396 ) ) ;
#8911 = CARTESIAN_POINT ( 'NONE',  ( -9.506476073891887424, 72.54341816039358548, -11.73172419143293865 ) ) ;
#8912 = DIRECTION ( 'NONE',  ( -1.000000000000000000, -0.000000000000000000, -0.000000000000000000 ) ) ;
#8913 = CARTESIAN_POINT ( 'NONE',  ( -78.00000000000001421, 50.75735931288069480, -4.242637315201482906 ) ) ;
#8914 = DIRECTION ( 'NONE',  ( 0.000000000000000000, 0.000000000000000000, 1.000000000000000000 ) ) ;
#8915 = CARTESIAN_POINT ( 'NONE',  ( -71.75000000204840944, 65.69163855873948421, -25.81189881250000440 ) ) ;
#8916 = ORIENTED_EDGE ( 'NONE', *, *, #5414, .F. ) ;
#8917 = CARTESIAN_POINT ( 'NONE',  ( -73.90625000409680467, 80.00000000000001421, 10.35533905932737397 ) ) ;
#8918 = DIRECTION ( 'NONE',  ( 1.000000000000000000, 0.000000000000000000, 0.000000000000000000 ) ) ;
#8919 = DIRECTION ( 'NONE',  ( -1.000000000000000000, -0.000000000000000000, -0.000000000000000000 ) ) ;
#8920 = VECTOR ( 'NONE', #7723, 1000.000000000000000 ) ;
#8921 = CARTESIAN_POINT ( 'NONE',  ( -52.88146049032556562, 73.03766007303350705, 10.81102556547625149 ) ) ;
#8922 = ORIENTED_EDGE ( 'NONE', *, *, #839, .F. ) ;
#8923 = CARTESIAN_POINT ( 'NONE',  ( -78.00000000000001421, 63.48528137423857487, 9.985284746156350977 ) ) ;
#8924 = AXIS2_PLACEMENT_3D ( 'NONE', #7393, #3975, #5723 ) ;
#8925 = CARTESIAN_POINT ( 'NONE',  ( -69.14775524013775510, 50.25531755529721778, 1.611686515444774148 ) ) ;
#8926 = EDGE_CURVE ( 'NONE', #2315, #11218, #8706, .T. ) ;
#8927 = EDGE_CURVE ( 'NONE', #2139, #7152, #2431, .T. ) ;
#8928 = B_SPLINE_CURVE_WITH_KNOTS ( 'NONE', 3,
 ( #926, #1887, #11045, #1173, #10089, #5742 ),
 .UNSPECIFIED., .F., .F.,
 ( 4, 2, 4 ),
 ( 0.005150343764683555127, 0.006610526168996384844, 0.008070708573309213693 ),
 .UNSPECIFIED. ) ;
#8929 = DIRECTION ( 'NONE',  ( 0.000000000000000000, 0.000000000000000000, -1.000000000000000000 ) ) ;
#8930 = CARTESIAN_POINT ( 'NONE',  ( -69.52691976458234535, 34.01892180236649921, 2.749684864678113794 ) ) ;
#8931 = CYLINDRICAL_SURFACE ( 'NONE', #2133, 1.499999999999999556 ) ;
#8932 = CARTESIAN_POINT ( 'NONE',  ( -79.53125000204838102, 55.00000000000000000, -25.81189881249999729 ) ) ;
#8933 = LINE ( 'NONE', #7091, #7282 ) ;
#8934 = ORIENTED_EDGE ( 'NONE', *, *, #7678, .T. ) ;
#8935 = AXIS2_PLACEMENT_3D ( 'NONE', #594, #6791, #7856 ) ;
#8936 = CARTESIAN_POINT ( 'NONE',  ( -72.12500000409677625, 55.00000000000000000, 24.99999999999999645 ) ) ;
#8937 = EDGE_LOOP ( 'NONE', ( #1068, #11209 ) ) ;
#8938 = CARTESIAN_POINT ( 'NONE',  ( 22.80989338617025552, 77.89797702579812722, 10.04169729082317986 ) ) ;
#8939 = CARTESIAN_POINT ( 'NONE',  ( -59.79192388697324390, 53.29971140327118206, 6.792174639222999133 ) ) ;
#8940 = CARTESIAN_POINT ( 'NONE',  ( -80.00000000000001421, 50.75735931288069480, -12.72791868944003824 ) ) ;
#8941 = CARTESIAN_POINT ( 'NONE',  ( -78.59375000000001421, 44.64466094067047663, -24.99999999999782219 ) ) ;
#8942 = EDGE_CURVE ( 'NONE', #2575, #6052, #488, .T. ) ;
#8943 = EDGE_CURVE ( 'NONE', #8561, #2740, #11049, .T. ) ;
#8944 = EDGE_CURVE ( 'NONE', #760, #8109, #11440, .T. ) ;
#8945 = CARTESIAN_POINT ( 'NONE',  ( -77.93750000000005684, 72.67766952966363192, 17.67766952966363547 ) ) ;
#8946 = CARTESIAN_POINT ( 'NONE',  ( -72.68750000204839523, 44.30836144126052289, 25.81189881250000795 ) ) ;
#8947 = AXIS2_PLACEMENT_3D ( 'NONE', #9493, #323, #11154 ) ;
#8948 = VERTEX_POINT ( 'NONE', #7156 ) ;
#8949 = SURFACE_SIDE_STYLE ('',( #6320 ) ) ;
#8950 = CARTESIAN_POINT ( 'NONE',  ( -78.68750000204839523, 65.69163855873949842, 25.81189881250000440 ) ) ;
#8951 = CARTESIAN_POINT ( 'NONE',  ( 14.99999999999999645, 5.000000000000000000, 30.00000000000000711 ) ) ;
#8952 = EDGE_CURVE ( 'NONE', #9962, #8176, #6375, .T. ) ;
#8953 = EDGE_CURVE ( 'NONE', #8979, #5671, #3543, .T. ) ;
#8954 = CARTESIAN_POINT ( 'NONE',  ( 37.00000000000000000, 55.00000000000000000, 0.000000000000000000 ) ) ;
#8955 = DIRECTION ( 'NONE',  ( -0.000000000000000000, -0.000000000000000000, 1.000000000000000000 ) ) ;
#8956 = VECTOR ( 'NONE', #9844, 1000.000000000000000 ) ;
#8957 = CARTESIAN_POINT ( 'NONE',  ( -74.99999999999995737, 40.75327862118771804, 20.61280595097384349 ) ) ;
#8958 = EDGE_CURVE ( 'NONE', #6004, #7332, #4923, .T. ) ;
#8959 = VERTEX_POINT ( 'NONE', #10780 ) ;
#8960 = CARTESIAN_POINT ( 'NONE',  ( -17.00978866326984473, 58.05348413988616585, 3.972925965357411826 ) ) ;
#8961 = DIRECTION ( 'NONE',  ( -1.000000000000000000, -0.000000000000000000, -0.000000000000000000 ) ) ;
#8962 = EDGE_LOOP ( 'NONE', ( #8753, #9794 ) ) ;
#8963 = CARTESIAN_POINT ( 'NONE',  ( -21.83980934632623772, 59.12499887129341403, 20.69724524603370597 ) ) ;
#8964 = CARTESIAN_POINT ( 'NONE',  ( -78.40625000204838102, 29.18810118750000271, 4.741568889096522788E-15 ) ) ;
#8965 = AXIS2_PLACEMENT_3D ( 'NONE', #4134, #7797, #8814 ) ;
#8966 = ORIENTED_EDGE ( 'NONE', *, *, #5408, .T. ) ;
#8967 = CARTESIAN_POINT ( 'NONE',  ( -72.96875000204838102, 73.25176868561975141, 18.25176868561974075 ) ) ;
#8968 = LINE ( 'NONE', #10802, #10049 ) ;
#8969 = EDGE_LOOP ( 'NONE', ( #1847, #4787, #10775 ) ) ;
#8970 = CARTESIAN_POINT ( 'NONE',  ( 9.999999999999994671, -30.00000000000000000, -10.00000000000000000 ) ) ;
#8971 = CARTESIAN_POINT ( 'NONE',  ( 5.616230220889759479E-16, -17.00000000000000000, 4.171999999999999709 ) ) ;
#8972 = CARTESIAN_POINT ( 'NONE',  ( -58.75094087149691546, 58.30862544132050118, 6.191974367482877106 ) ) ;
#8973 = EDGE_LOOP ( 'NONE', ( #559, #11783 ) ) ;
#8974 = CARTESIAN_POINT ( 'NONE',  ( -14.52231952541034943, 75.43188300159135906, 5.490993919093054565 ) ) ;
#8975 = CARTESIAN_POINT ( 'NONE',  ( -3.477628190354089099, 49.49309465598528845, -20.46958112014059950 ) ) ;
#8976 = FACE_OUTER_BOUND ( 'NONE', #6696, .T. ) ;
#8977 = CARTESIAN_POINT ( 'NONE',  ( -78.00000000000000000, 55.00000000000000000, -21.50000000000000000 ) ) ;
#8978 = CARTESIAN_POINT ( 'NONE',  ( -78.00000000000002842, 54.99999999999998579, 16.97056612039490986 ) ) ;
#8979 = VERTEX_POINT ( 'NONE', #7098 ) ;
#8980 = CARTESIAN_POINT ( 'NONE',  ( -78.00000000000001421, 71.97056274847716395, 3.371917795327861178E-06 ) ) ;
#8981 = CARTESIAN_POINT ( 'NONE',  ( -68.34104732181950226, 33.99448141944334623, 0.006743540747238889813 ) ) ;
#8982 = FACE_OUTER_BOUND ( 'NONE', #7198, .T. ) ;
#8983 = CARTESIAN_POINT ( 'NONE',  ( -42.66281101964754896, 63.04450918361814615, -19.42252581123130639 ) ) ;
#8984 = VECTOR ( 'NONE', #10243, 1000.000000000000000 ) ;
#8985 = VERTEX_POINT ( 'NONE', #2591 ) ;
#8986 = CARTESIAN_POINT ( 'NONE',  ( 73.00000000000000000, 97.00000000000000000, -9.797174393178809880E-16 ) ) ;
#8987 = AXIS2_PLACEMENT_3D ( 'NONE', #11662, #2627, #9809 ) ;
#8988 = CARTESIAN_POINT ( 'NONE',  ( -78.59375000409677625, 80.00000000000001421, -10.35533905932737753 ) ) ;
#8989 = ORIENTED_EDGE ( 'NONE', *, *, #1408, .T. ) ;
#8990 = DIRECTION ( 'NONE',  ( -1.000000000000000000, 0.000000000000000000, 0.000000000000000000 ) ) ;
#8991 = CARTESIAN_POINT ( 'NONE',  ( 6.288736434038950662, 50.50500022705934811, 2.214244300018950895 ) ) ;
#8992 = AXIS2_PLACEMENT_3D ( 'NONE', #993, #11107, #9322 ) ;
#8993 = CARTESIAN_POINT ( 'NONE',  ( -77.65625000204838102, 80.81189881250000440, -1.580522963032174394E-15 ) ) ;
#8994 = CARTESIAN_POINT ( 'NONE',  ( -74.93750000204839523, 65.69163855873948421, -25.81189881250000440 ) ) ;
#8995 = CIRCLE ( 'NONE', #10509, 1.500000000000001332 ) ;
#8996 = ORIENTED_EDGE ( 'NONE', *, *, #6959, .F. ) ;
#8997 = DIRECTION ( 'NONE',  ( 0.000000000000000000, 0.000000000000000000, 1.000000000000000000 ) ) ;
#8998 = VERTEX_POINT ( 'NONE', #11800 ) ;
#8999 = CARTESIAN_POINT ( 'NONE',  ( -0.6792758137180379130, 53.69893887388462872, -4.838731147744609551 ) ) ;
#9000 = CARTESIAN_POINT ( 'NONE',  ( 6.077181813707832170, 41.04144508200626262, -1.373101212108361002 ) ) ;
#9001 = CARTESIAN_POINT ( 'NONE',  ( -78.31250000204839523, 29.18810118750000981, 10.69163855873950020 ) ) ;
#9002 = LINE ( 'NONE', #5236, #9700 ) ;
#9003 = DIRECTION ( 'NONE',  ( 0.000000000000000000, 0.000000000000000000, 1.000000000000000000 ) ) ;
#9004 = CARTESIAN_POINT ( 'NONE',  ( -72.87500000204838102, 65.69163855873949842, 25.81189881250000084 ) ) ;
#9005 = ORIENTED_EDGE ( 'NONE', *, *, #8958, .T. ) ;
#9006 = CARTESIAN_POINT ( 'NONE',  ( -73.53125000204839523, 36.74823131438024859, -18.25176868561973720 ) ) ;
#9007 = CARTESIAN_POINT ( 'NONE',  ( -80.00000000000000000, 55.00000000000000000, 21.50000000000000000 ) ) ;
#9008 = CIRCLE ( 'NONE', #3644, 1.500000000000001332 ) ;
#9009 = FACE_OUTER_BOUND ( 'NONE', #605, .T. ) ;
#9010 = CARTESIAN_POINT ( 'NONE',  ( -51.87153091508479719, 55.00409571353115012, 0.001995793859737243683 ) ) ;
#9011 = FACE_OUTER_BOUND ( 'NONE', #1053, .T. ) ;
#9012 = AXIS2_PLACEMENT_3D ( 'NONE', #5730, #10260, #2118 ) ;
#9013 = ORIENTED_EDGE ( 'NONE', *, *, #4777, .F. ) ;
#9014 = AXIS2_PLACEMENT_3D ( 'NONE', #7690, #11324, #5898 ) ;
#9015 = CARTESIAN_POINT ( 'NONE',  ( -10.59643185551853151, 59.93469145766130879, -0.8217785073578240951 ) ) ;
#9016 = EDGE_CURVE ( 'NONE', #8530, #9830, #6798, .T. ) ;
#9017 = CARTESIAN_POINT ( 'NONE',  ( -55.73751408985167899, 71.24607175163586703, 13.33484869932101269 ) ) ;
#9018 = ORIENTED_EDGE ( 'NONE', *, *, #8425, .T. ) ;
#9019 = CARTESIAN_POINT ( 'NONE',  ( -36.18906244468503530, 38.22373822049622305, -12.89330079981896482 ) ) ;
#9020 = CARTESIAN_POINT ( 'NONE',  ( -74.93750000204839523, 65.69163855873948421, -25.81189881250000440 ) ) ;
#9021 = AXIS2_PLACEMENT_3D ( 'NONE', #1098, #9365, #379 ) ;
#9022 = CIRCLE ( 'NONE', #10346, 1.500000000000001332 ) ;
#9023 = ORIENTED_EDGE ( 'NONE', *, *, #4409, .F. ) ;
#9024 = CARTESIAN_POINT ( 'NONE',  ( -73.81250000204839523, 29.18810118750000626, -10.69163855873949309 ) ) ;
#9025 = CARTESIAN_POINT ( 'NONE',  ( 36.99999999999999289, 45.00000000000001421, 1.224646799147351679E-15 ) ) ;
#9026 = SURFACE_SIDE_STYLE ('',( #3454 ) ) ;
#9027 = EDGE_CURVE ( 'NONE', #11066, #8197, #1744, .T. ) ;
#9028 = DIRECTION ( 'NONE',  ( 1.000000000000000000, 0.000000000000000000, 0.000000000000000000 ) ) ;
#9029 = CARTESIAN_POINT ( 'NONE',  ( 0.000000000000000000, 0.000000000000000000, -3.482085714285714229 ) ) ;
#9030 = CARTESIAN_POINT ( 'NONE',  ( -7.170201598857286029, 54.99827432856260145, 0.003516170034810423960 ) ) ;
#9031 = EDGE_LOOP ( 'NONE', ( #9710, #4468, #3977, #11578 ) ) ;
#9032 = CARTESIAN_POINT ( 'NONE',  ( -7.452025537132175970, 67.52141018531283123, -16.88433180000173195 ) ) ;
#9033 = CARTESIAN_POINT ( 'NONE',  ( -42.03064326886630653, 53.96872019721284630, -20.99365203016559178 ) ) ;
#9034 = CARTESIAN_POINT ( 'NONE',  ( -78.00000000000000000, 54.99999999999999289, 0.000000000000000000 ) ) ;
#9035 = CARTESIAN_POINT ( 'NONE',  ( -75.59375000000005684, 44.64466094067241642, -24.99999999999965539 ) ) ;
#9036 = FACE_OUTER_BOUND ( 'NONE', #2961, .T. ) ;
#9037 = ORIENTED_EDGE ( 'NONE', *, *, #1824, .F. ) ;
#9038 = DIRECTION ( 'NONE',  ( -1.000000000000000000, 0.000000000000000000, 0.000000000000000000 ) ) ;
#9039 = CARTESIAN_POINT ( 'NONE',  ( 0.000000000000000000, 0.000000000000000000, -0.5394676594665810399 ) ) ;
#9040 = FACE_BOUND ( 'NONE', #5871, .T. ) ;
#9041 = ORIENTED_EDGE ( 'NONE', *, *, #5370, .F. ) ;
#9042 = CARTESIAN_POINT ( 'NONE',  ( 0.000000000000000000, 0.000000000000000000, -0.3755037691048591086 ) ) ;
#9043 = CARTESIAN_POINT ( 'NONE',  ( -57.87010688772392086, 58.05147143109211072, 3.974243011944121662 ) ) ;
#9044 = ORIENTED_EDGE ( 'NONE', *, *, #447, .T. ) ;
#9045 = EDGE_CURVE ( 'NONE', #306, #4164, #9887, .T. ) ;
#9046 = FACE_OUTER_BOUND ( 'NONE', #7789, .T. ) ;
#9047 = DIRECTION ( 'NONE',  ( -0.000000000000000000, -0.000000000000000000, -1.000000000000000000 ) ) ;
#9048 = CARTESIAN_POINT ( 'NONE',  ( -74.18750000204838102, 44.30836144126053000, 25.81189881250000795 ) ) ;
#9049 = CARTESIAN_POINT ( 'NONE',  ( -79.53125000204838102, 55.00000000000000000, -25.81189881249999729 ) ) ;
#9050 = EDGE_LOOP ( 'NONE', ( #8238, #9362, #1616, #7940 ) ) ;
#9051 = CARTESIAN_POINT ( 'NONE',  ( -75.21875000204839523, 29.18810118750000271, 4.741568889096522788E-15 ) ) ;
#9052 = ORIENTED_EDGE ( 'NONE', *, *, #8779, .T. ) ;
#9053 = CARTESIAN_POINT ( 'NONE',  ( 4.235829868893991268, 66.01841521325340523, 22.44289296408692991 ) ) ;
#9054 = CARTESIAN_POINT ( 'NONE',  ( 16.79375990066182922, 56.83099525978803257, 13.97545931189135793 ) ) ;
#9055 = CARTESIAN_POINT ( 'NONE',  ( -78.40625000204839523, 36.74823131438026280, 18.25176868561974786 ) ) ;
#9056 = CARTESIAN_POINT ( 'NONE',  ( -80.00000000000001421, 46.51471862576140381, -8.485278002320759683 ) ) ;
#9057 = CARTESIAN_POINT ( 'NONE',  ( 1.474044695502842117, 65.07161681208872039, -19.55923518678806161 ) ) ;
#9058 = EDGE_LOOP ( 'NONE', ( #8185, #4798 ) ) ;
#9059 = EDGE_CURVE ( 'NONE', #642, #4918, #8353, .T. ) ;
#9060 = DIRECTION ( 'NONE',  ( -1.000000000000000000, 0.000000000000000000, 0.000000000000000000 ) ) ;
#9061 = CARTESIAN_POINT ( 'NONE',  ( -75.68750000409677625, 72.67766952966368876, -17.67766952966368876 ) ) ;
#9062 = CARTESIAN_POINT ( 'NONE',  ( -36.87377965891732146, 50.66043048872463572, -2.505278942661100849 ) ) ;
#9063 = EDGE_CURVE ( 'NONE', #6726, #2603, #9002, .T. ) ;
#9064 = DIRECTION ( 'NONE',  ( -1.000000000000000000, 0.000000000000000000, 0.000000000000000000 ) ) ;
#9065 = CARTESIAN_POINT ( 'NONE',  ( -37.56959447096606652, 54.99363160768596259, -0.01863072254107098896 ) ) ;
#9066 = SHAPE_DEFINITION_REPRESENTATION ( #11212, #3715 ) ;
#9067 = CYLINDRICAL_SURFACE ( 'NONE', #4615, 9.999999999999987566 ) ;
#9068 = CARTESIAN_POINT ( 'NONE',  ( -24.01777539311168397, 52.49472557160137143, 4.339384516595543140 ) ) ;
#9069 = EDGE_LOOP ( 'NONE', ( #5961, #1283 ) ) ;
#9070 = AXIS2_PLACEMENT_3D ( 'NONE', #8913, #9804, #6112 ) ;
#9071 = EDGE_CURVE ( 'NONE', #8766, #2363, #7604, .T. ) ;
#9072 = CARTESIAN_POINT ( 'NONE',  ( -62.73530513678402087, 48.89572068339310107, 20.11073150603193938 ) ) ;
#9073 = VERTEX_POINT ( 'NONE', #6313 ) ;
#9074 = CARTESIAN_POINT ( 'NONE',  ( 4.329456757236127551, 33.97246960341611555, -0.0004353087921988608999 ) ) ;
#9075 = CARTESIAN_POINT ( 'NONE',  ( -72.96875000204838102, 73.25176868561975141, 18.25176868561974075 ) ) ;
#9076 = EDGE_LOOP ( 'NONE', ( #4993, #2338, #10553, #10604 ) ) ;
#9077 = CARTESIAN_POINT ( 'NONE',  ( -73.25000000204838102, 80.81189881250001861, -10.69163855873949132 ) ) ;
#9078 = CARTESIAN_POINT ( 'NONE',  ( -28.67054321954914542, 35.57240153874681710, 8.046710727719679213 ) ) ;
#9079 = EDGE_LOOP ( 'NONE', ( #9052, #4151 ) ) ;
#9080 = LINE ( 'NONE', #8970, #3235 ) ;
#9081 = EDGE_CURVE ( 'NONE', #9521, #7673, #1261, .T. ) ;
#9082 = CARTESIAN_POINT ( 'NONE',  ( -61.66652652224714615, 54.99971167242890147, 7.011010121665977479 ) ) ;
#9083 = ORIENTED_EDGE ( 'NONE', *, *, #11821, .T. ) ;
#9084 = CARTESIAN_POINT ( 'NONE',  ( -4.274947514841225704, 57.05942961895281229, -21.01658053370092816 ) ) ;
#9085 = EDGE_CURVE ( 'NONE', #6717, #193, #10738, .T. ) ;
#9086 = CARTESIAN_POINT ( 'NONE',  ( 2.881307801134362023, 34.60859193927083055, -5.107160905361891601 ) ) ;
#9087 = CARTESIAN_POINT ( 'NONE',  ( 4.999999999999999112, -0.4878135028931883110, -6.100000000000002309 ) ) ;
#9088 = CYLINDRICAL_SURFACE ( 'NONE', #5360, 1.500000000000000000 ) ;
#9089 = DIRECTION ( 'NONE',  ( 0.8191520442889885789, 0.000000000000000000, 0.5735764363510507113 ) ) ;
#9090 = ORIENTED_EDGE ( 'NONE', *, *, #8779, .F. ) ;
#9091 = CARTESIAN_POINT ( 'NONE',  ( -20.00000000000003197, -57.00000000000000000, 5.000000000000000000 ) ) ;
#9092 = CARTESIAN_POINT ( 'NONE',  ( -37.90726342759032264, 55.01040348274680269, 0.01273213325553751787 ) ) ;
#9093 = CARTESIAN_POINT ( 'NONE',  ( -36.26619597527190564, 52.35453385845364238, -4.245986690839498756 ) ) ;
#9094=STYLED_ITEM('',(#11874),#912);
#9095 = CARTESIAN_POINT ( 'NONE',  ( -80.00000000000001421, 50.75735931288069480, -11.22791868944003824 ) ) ;
#9096 = EDGE_CURVE ( 'NONE', #9224, #9431, #8883, .T. ) ;
#9097 = LINE ( 'NONE', #3529, #693 ) ;
#9098 = ORIENTED_EDGE ( 'NONE', *, *, #10541, .T. ) ;
#9099 = DIRECTION ( 'NONE',  ( -1.000000000000000000, -0.000000000000000000, -0.000000000000000000 ) ) ;
#9100 = FACE_OUTER_BOUND ( 'NONE', #4852, .T. ) ;
#9101 = DIRECTION ( 'NONE',  ( 1.000000000000000000, 6.033820786006286457E-17, 0.000000000000000000 ) ) ;
#9102 = CARTESIAN_POINT ( 'NONE',  ( -73.90625000204838102, 29.18810118750000271, 4.741568889096522788E-15 ) ) ;
#9103 = CARTESIAN_POINT ( 'NONE',  ( -79.06250000204839523, 80.81189881250001861, 10.69163855873948599 ) ) ;
#9104 = AXIS2_PLACEMENT_3D ( 'NONE', #6946, #6219, #8850 ) ;
#9105 = ORIENTED_EDGE ( 'NONE', *, *, #4089, .F. ) ;
#9106 = CARTESIAN_POINT ( 'NONE',  ( -75.50000000204840944, 44.30836144126053000, 25.81189881250000795 ) ) ;
#9107 = VERTEX_POINT ( 'NONE', #719 ) ;
#9108 = CARTESIAN_POINT ( 'NONE',  ( 17.59011022552445880, 73.70148073974591796, 16.59389287537950963 ) ) ;
#9109 = CARTESIAN_POINT ( 'NONE',  ( -18.12197315986341550, 62.20417759841708261, 12.01780937852947595 ) ) ;
#9110 =( GEOMETRIC_REPRESENTATION_CONTEXT ( 3 ) GLOBAL_UNCERTAINTY_ASSIGNED_CONTEXT ( ( #3832 ) ) GLOBAL_UNIT_ASSIGNED_CONTEXT ( ( #11105, #9202, #1826 ) ) REPRESENTATION_CONTEXT ( 'NONE', 'WORKASPACE' ) );
#9111 = CARTESIAN_POINT ( 'NONE',  ( 39.99999999999999289, 55.00000000000000000, -24.99999999999999645 ) ) ;
#9112 = CARTESIAN_POINT ( 'NONE',  ( -2.500000000000000000, 3.061616997868383141E-16, -4.696360911962001339 ) ) ;
#9113 = CARTESIAN_POINT ( 'NONE',  ( -79.43750000204838102, 55.00000000000000000, -25.81189881249999729 ) ) ;
#9114 = ORIENTED_EDGE ( 'NONE', *, *, #3450, .F. ) ;
#9115 = DIRECTION ( 'NONE',  ( 0.000000000000000000, 0.000000000000000000, 1.000000000000000000 ) ) ;
#9116 = CARTESIAN_POINT ( 'NONE',  ( -76.43750000409679046, 37.32233047033631124, 17.67766952966369232 ) ) ;
#9117 = LINE ( 'NONE', #1, #3647 ) ;
#9118 = CARTESIAN_POINT ( 'NONE',  ( -23.75939059330988457, 54.98844314865997518, 0.02356513468685287119 ) ) ;
#9119 = PRODUCT_CONTEXT ( 'NONE', #5325, 'mechanical' ) ;
#9120 = CARTESIAN_POINT ( 'NONE',  ( -17.17085726908380394, 73.30622707836364782, -12.21665692408397241 ) ) ;
#9121 = AXIS2_PLACEMENT_3D ( 'NONE', #7740, #9529, #475 ) ;
#9122 = CARTESIAN_POINT ( 'NONE',  ( -8.462009850179832426, 59.33805624513391308, -2.507821275865560029 ) ) ;
#9123 = AXIS2_PLACEMENT_3D ( 'NONE', #2931, #9156, #10227 ) ;
#9124 = VERTEX_POINT ( 'NONE', #4391 ) ;
#9125 = CARTESIAN_POINT ( 'NONE',  ( 2.712167343862819546, 4.207632145829744985, 4.204248033696719733E-15 ) ) ;
#9126 = EDGE_LOOP ( 'NONE', ( #6570, #8058, #6133, #8126, #10673 ) ) ;
#9127 = ADVANCED_FACE ( 'NONE', ( #8044 ), #4621, .F. ) ;
#9128 = CARTESIAN_POINT ( 'NONE',  ( -12.81092923270300865, 75.46953867936616689, -5.507006106411301616 ) ) ;
#9129 = CARTESIAN_POINT ( 'NONE',  ( -72.03125000204838102, 55.00000000000000000, -25.81189881249999729 ) ) ;
#9130 = VECTOR ( 'NONE', #6774, 1000.000000000000000 ) ;
#9131 = PRESENTATION_LAYER_ASSIGNMENT (  '', '', ( #3589 ) ) ;
#9132 = EDGE_LOOP ( 'NONE', ( #8781, #8617 ) ) ;
#9133 = CARTESIAN_POINT ( 'NONE',  ( -76.34375000204839523, 73.25176868561975141, -18.25176868561974430 ) ) ;
#9134 = CARTESIAN_POINT ( 'NONE',  ( -32.17314280228392676, 34.29902663375150240, -4.109485608336678197 ) ) ;
#9135 = EDGE_CURVE ( 'NONE', #193, #8038, #50, .T. ) ;
#9136 =( BOUNDED_CURVE ( )  B_SPLINE_CURVE ( 2, ( #9840, #9955, #2658, #10788, #7107, #8053, #11696, #3497, #728 ),
 .UNSPECIFIED., .F., .T. ) 
 B_SPLINE_CURVE_WITH_KNOTS ( ( 3, 2, 2, 2, 3 ),
 ( 0.1666666666666667962, 0.1875000000000001665, 0.2083333333333335369, 0.2291666666666668517, 0.2500000000000002220 ),
 .UNSPECIFIED. ) 
 CURVE ( )  GEOMETRIC_REPRESENTATION_ITEM ( )  RATIONAL_B_SPLINE_CURVE ( ( 0.9999999999999994449, 0.9238795325112872936, 1.000000000000000000, 0.9238795325112867385, 1.000000000000000000, 0.9238795325112867385, 1.000000000000000000, 0.9238795325112859613, 1.000000000000000888 ) ) 
 REPRESENTATION_ITEM ( '' )  );
#9137 = EDGE_LOOP ( 'NONE', ( #11011, #9193 ) ) ;
#9138 = CARTESIAN_POINT ( 'NONE',  ( 0.000000000000000000, -57.00000000000000000, -5.000000000000000000 ) ) ;
#9139 = CARTESIAN_POINT ( 'NONE',  ( -64.00030959431065014, 52.31932374249372941, 6.472111605756746933 ) ) ;
#9140 = AXIS2_PLACEMENT_3D ( 'NONE', #6907, #11489, #4259 ) ;
#9141 = ORIENTED_EDGE ( 'NONE', *, *, #9821, .F. ) ;
#9142 = CARTESIAN_POINT ( 'NONE',  ( -40.69731036757077192, 53.96875818098316557, -20.99256918425749063 ) ) ;
#9143 = CARTESIAN_POINT ( 'NONE',  ( 1.697306494461763959, 35.98764835359665426, -8.991780390316415961 ) ) ;
#9144 = CARTESIAN_POINT ( 'NONE',  ( -72.96875000409677625, 44.64466094067281432, -25.00000000000019540 ) ) ;
#9145 = DIRECTION ( 'NONE',  ( -0.000000000000000000, -1.000000000000000000, -0.000000000000000000 ) ) ;
#9146 = DIRECTION ( 'NONE',  ( -1.000000000000000000, -0.000000000000000000, -0.000000000000000000 ) ) ;
#9147 = CARTESIAN_POINT ( 'NONE',  ( -80.00000000000002842, 42.27207793864211283, -4.242637315201479353 ) ) ;
#9148 = ORIENTED_EDGE ( 'NONE', *, *, #10688, .T. ) ;
#9149 = DIRECTION ( 'NONE',  ( -1.000000000000000000, 0.000000000000000000, 0.000000000000000000 ) ) ;
#9150 = CARTESIAN_POINT ( 'NONE',  ( -31.38106053236869286, 55.00524807308060105, -0.001787053225003424348 ) ) ;
#9151 = CARTESIAN_POINT ( 'NONE',  ( -31.01894826520979365, 49.99999999999997868, -0.6617035227858814039 ) ) ;
#9152 = DIRECTION ( 'NONE',  ( -1.000000000000000000, -0.000000000000000000, -0.000000000000000000 ) ) ;
#9153 = CARTESIAN_POINT ( 'NONE',  ( -78.21875000409677625, 65.35533905932734910, 25.00000000000002132 ) ) ;
#9154 = AXIS2_PLACEMENT_3D ( 'NONE', #21, #8244, #3571 ) ;
#9155 = ORIENTED_EDGE ( 'NONE', *, *, #2646, .F. ) ;
#9156 = DIRECTION ( 'NONE',  ( -1.000000000000000000, -0.000000000000000000, -0.000000000000000000 ) ) ;
#9157 = EDGE_CURVE ( 'NONE', #2610, #11481, #314, .T. ) ;
#9158 = DIRECTION ( 'NONE',  ( -1.000000000000000000, -0.000000000000000000, -0.000000000000000000 ) ) ;
#9159 = CARTESIAN_POINT ( 'NONE',  ( 52.99999999999999289, 101.0000000000000000, -9.797174393178809880E-16 ) ) ;
#9160 = CARTESIAN_POINT ( 'NONE',  ( -20.20056265816597829, 75.75497107137435648, -13.94119571728393225 ) ) ;
#9161 = CARTESIAN_POINT ( 'NONE',  ( -78.21875000204839523, 36.74823131438024859, -18.25176868561973720 ) ) ;
#9162 = ORIENTED_EDGE ( 'NONE', *, *, #6760, .T. ) ;
#9163 = DIRECTION ( 'NONE',  ( -6.033820786006286457E-17, 1.000000000000000000, 0.000000000000000000 ) ) ;
#9164 = ORIENTED_EDGE ( 'NONE', *, *, #4012, .T. ) ;
#9165 = CARTESIAN_POINT ( 'NONE',  ( -6.128719672236011107, 58.04896597338179021, -3.976206575877460736 ) ) ;
#9166 = VECTOR ( 'NONE', #11220, 1000.000000000000000 ) ;
#9167 = CARTESIAN_POINT ( 'NONE',  ( -27.16357883943494400, 43.30581957307868635, 7.809306310971448895 ) ) ;
#9168 = ADVANCED_FACE ( 'NONE', ( #8395, #954 ), #4866, .T. ) ;
#9169 = LINE ( 'NONE', #953, #5196 ) ;
#9170 = CARTESIAN_POINT ( 'NONE',  ( -75.00000000000002842, 79.21399255846120013, -7.542952894479948434 ) ) ;
#9171 = DIRECTION ( 'NONE',  ( 0.000000000000000000, -0.000000000000000000, -1.000000000000000000 ) ) ;
#9172 = AXIS2_PLACEMENT_3D ( 'NONE', #9978, #1774, #5440 ) ;
#9173 = VECTOR ( 'NONE', #4882, 1000.000000000000000 ) ;
#9174 = ORIENTED_EDGE ( 'NONE', *, *, #3084, .F. ) ;
#9175 = CARTESIAN_POINT ( 'NONE',  ( -79.71875000000001421, 80.00000000000001421, -10.35533905932737753 ) ) ;
#9176 = CARTESIAN_POINT ( 'NONE',  ( -78.12500000409677625, 55.00000000000000000, 24.99999999999999645 ) ) ;
#9177 = CYLINDRICAL_SURFACE ( 'NONE', #9766, 24.99999999999999645 ) ;
#9178 = CARTESIAN_POINT ( 'NONE',  ( -55.09748469029145923, 54.99365593231603810, -0.01917390278371958537 ) ) ;
#9179 = PRODUCT_CONTEXT ( 'NONE', #10888, 'mechanical' ) ;
#9180 = AXIS2_PLACEMENT_3D ( 'NONE', #7596, #391, #6821 ) ;
#9181 = CARTESIAN_POINT ( 'NONE',  ( -21.27969014566767569, 76.63537834043187047, -4.004875479550875639 ) ) ;
#9182 = CARTESIAN_POINT ( 'NONE',  ( -23.62122360972324842, 52.78556759016737487, 4.494981739694955181 ) ) ;
#9183 = ORIENTED_EDGE ( 'NONE', *, *, #2058, .F. ) ;
#9184 = CARTESIAN_POINT ( 'NONE',  ( -76.25000000000000000, 55.00000000000000000, 24.99999999999999645 ) ) ;
#9185 = ORIENTED_EDGE ( 'NONE', *, *, #1627, .T. ) ;
#9186 = CARTESIAN_POINT ( 'NONE',  ( -8.785358865379802040, 67.52185545713140868, -16.88477868139494831 ) ) ;
#9187 = CARTESIAN_POINT ( 'NONE',  ( -72.78125000204838102, 55.00000000000000000, 25.81189881249999729 ) ) ;
#9188 = ORIENTED_EDGE ( 'NONE', *, *, #307, .F. ) ;
#9189 = CARTESIAN_POINT ( 'NONE',  ( -74.65625000204838102, 80.81189881250000440, -1.580522963032174394E-15 ) ) ;
#9190 = CARTESIAN_POINT ( 'NONE',  ( -40.92935782463053584, 57.05919160630219977, -20.93299540428984429 ) ) ;
#9191 = AXIS2_PLACEMENT_3D ( 'NONE', #7162, #10787, #9780 ) ;
#9192 = DIRECTION ( 'NONE',  ( -1.000000000000000000, -0.000000000000000000, -0.000000000000000000 ) ) ;
#9193 = ORIENTED_EDGE ( 'NONE', *, *, #2286, .T. ) ;
#9194 = AXIS2_PLACEMENT_3D ( 'NONE', #9395, #9456, #6719 ) ;
#9195 = CARTESIAN_POINT ( 'NONE',  ( -8.872461119604453827, 57.50149492254836758, -4.332372781979526799 ) ) ;
#9196 = CARTESIAN_POINT ( 'NONE',  ( 0.2748429140369315071, 38.70467982241823535, -13.38321124372595783 ) ) ;
#9197 = ORIENTED_EDGE ( 'NONE', *, *, #8196, .F. ) ;
#9198 = CARTESIAN_POINT ( 'NONE',  ( -26.18898619208348677, 42.10803998828228600, 16.77528611580634887 ) ) ;
#9199 = AXIS2_PLACEMENT_3D ( 'NONE', #5111, #1566, #10597 ) ;
#9200 = CARTESIAN_POINT ( 'NONE',  ( 2.595920079249742329, 34.88763922991881827, -6.102757042485290384 ) ) ;
#9201 = B_SPLINE_CURVE_WITH_KNOTS ( 'NONE', 3,
 ( #8224, #2825, #4810, #6559 ),
 .UNSPECIFIED., .F., .F.,
 ( 4, 4 ),
 ( 0.000000000000000000, 1.000000000000000000 ),
 .UNSPECIFIED. ) ;
#9202 =( NAMED_UNIT ( * ) PLANE_ANGLE_UNIT ( ) SI_UNIT ( $, .RADIAN. ) );
#9203 = DIRECTION ( 'NONE',  ( -1.000000000000000000, 0.000000000000000000, 0.000000000000000000 ) ) ;
#9204 = CARTESIAN_POINT ( 'NONE',  ( -78.00000000000000000, 59.99999999999998579, 0.000000000000000000 ) ) ;
#9205 = LINE ( 'NONE', #4654, #7099 ) ;
#9206 = VERTEX_POINT ( 'NONE', #5645 ) ;
#9207 =( BOUNDED_CURVE ( )  B_SPLINE_CURVE ( 2, ( #1781, #2751, #10041, #3825, #7491, #4905, #8376, #10344, #10284 ),
 .UNSPECIFIED., .F., .T. ) 
 B_SPLINE_CURVE_WITH_KNOTS ( ( 3, 2, 2, 2, 3 ),
 ( 0.2376281879409543607, 0.2574394709827818040, 0.2772507540246093027, 0.2970620370664368015, 0.3168733201082642448 ),
 .UNSPECIFIED. ) 
 CURVE ( )  GEOMETRIC_REPRESENTATION_ITEM ( )  RATIONAL_B_SPLINE_CURVE ( ( 0.9999999999999494849, 0.9238795325113373647, 1.000000000000000000, 0.9238795325112868495, 1.000000000000000000, 0.9238795325112868495, 1.000000000000000000, 0.9238795325112868495, 1.000000000000000000 ) ) 
 REPRESENTATION_ITEM ( '' )  );
#9208 = CARTESIAN_POINT ( 'NONE',  ( -76.25000000000000000, 55.00000000000000000, 24.99999999999999645 ) ) ;
#9209 = CARTESIAN_POINT ( 'NONE',  ( -30.50353493236575630, 55.00370654185008590, -0.001266073661171608069 ) ) ;
#9210 = PLANE ( 'NONE',  #1378 ) ;
#9211 = EDGE_CURVE ( 'NONE', #2686, #4040, #8275, .T. ) ;
#9212 = AXIS2_PLACEMENT_3D ( 'NONE', #11511, #10670, #440 ) ;
#9213 = CARTESIAN_POINT ( 'NONE',  ( 0.000000000000000000, 0.000000000000000000, -6.099999999999999645 ) ) ;
#9214 = CARTESIAN_POINT ( 'NONE',  ( -78.50000000409677625, 80.00000000000000000, -1.530808498934191324E-15 ) ) ;
#9215 = ORIENTED_EDGE ( 'NONE', *, *, #11645, .F. ) ;
#9216 = CARTESIAN_POINT ( 'NONE',  ( 11.81093755974026394, 42.10901286868706705, 16.77394813616862734 ) ) ;
#9217 = CARTESIAN_POINT ( 'NONE',  ( -72.40625000204838102, 29.18810118750000271, 4.741568889096522788E-15 ) ) ;
#9218 = CARTESIAN_POINT ( 'NONE',  ( 0.000000000000000000, 110.0000000000000000, 0.000000000000000000 ) ) ;
#9219 = CARTESIAN_POINT ( 'NONE',  ( 3.963041193916334137, 50.00000000000020606, 0.3308364528915549441 ) ) ;
#9220 = CARTESIAN_POINT ( 'NONE',  ( -72.59375000204838102, 36.74823131438026280, 18.25176868561974786 ) ) ;
#9221 = CARTESIAN_POINT ( 'NONE',  ( -75.12500000204838102, 44.30836144126050158, -25.81189881249999374 ) ) ;
#9222 = ORIENTED_EDGE ( 'NONE', *, *, #2572, .F. ) ;
#9223 = PLANE ( 'NONE',  #5581 ) ;
#9224 = VERTEX_POINT ( 'NONE', #11074 ) ;
#9225 =( NAMED_UNIT ( * ) SI_UNIT ( $, .STERADIAN. ) SOLID_ANGLE_UNIT ( ) );
#9226 = CARTESIAN_POINT ( 'NONE',  ( 14.46039494637405909, 51.34337453854569588, 13.61230544799882480 ) ) ;
#9227 = ADVANCED_FACE ( 'NONE', ( #3962 ), #2821, .F. ) ;
#9228 = DIRECTION ( 'NONE',  ( -1.000000000000000000, 0.000000000000000000, 0.000000000000000000 ) ) ;
#9229 = DIRECTION ( 'NONE',  ( 1.000000000000000000, 0.000000000000000000, 0.000000000000000000 ) ) ;
#9230 = DIRECTION ( 'NONE',  ( 0.000000000000000000, 0.000000000000000000, 1.000000000000000000 ) ) ;
#9231 = VERTEX_POINT ( 'NONE', #5770 ) ;
#9232 = CARTESIAN_POINT ( 'NONE',  ( 2.087481099544137350E-15, 50.52094453300079380, -17.04557674096337649 ) ) ;
#9233 = CARTESIAN_POINT ( 'NONE',  ( -72.78125000204839523, 73.25176868561975141, 18.25176868561974075 ) ) ;
#9234 = EDGE_CURVE ( 'NONE', #131, #9375, #763, .T. ) ;
#9235 = DIRECTION ( 'NONE',  ( 1.000000000000000000, 0.000000000000000000, 0.000000000000000000 ) ) ;
#9236 = CARTESIAN_POINT ( 'NONE',  ( -78.00000000000002842, 46.51471862576140381, 6.985284746156355418 ) ) ;
#9237 = CARTESIAN_POINT ( 'NONE',  ( -29.12853506694033356, 55.00558571566143229, 0.0002252870501606599272 ) ) ;
#9238 = ITEM_DEFINED_TRANSFORMATION ( 'NONE', 'NONE', #277,  #4738 ) ;
#9239 = CARTESIAN_POINT ( 'NONE',  ( -19.09301521363747511, 74.83539102382144392, -9.521771482395543273 ) ) ;
#9240 = CARTESIAN_POINT ( 'NONE',  ( -80.00000000000002842, 54.99999999999998579, 18.47056612039490986 ) ) ;
#9241 = EDGE_CURVE ( 'NONE', #1874, #4655, #4257, .T. ) ;
#9242 = VERTEX_POINT ( 'NONE', #6067 ) ;
#9243 = DIRECTION ( 'NONE',  ( 0.000000000000000000, 0.000000000000000000, 1.000000000000000000 ) ) ;
#9244 = CARTESIAN_POINT ( 'NONE',  ( -80.00000000000002842, 54.99999999999998579, 6.985284746156355418 ) ) ;
#9245 = ORIENTED_EDGE ( 'NONE', *, *, #8773, .F. ) ;
#9246 = CARTESIAN_POINT ( 'NONE',  ( 5.506399570602333426, 34.30736306936326230, 4.109392375493936100 ) ) ;
#9247 = CARTESIAN_POINT ( 'NONE',  ( -79.06250000204840944, 80.81189881250001861, -10.69163855873949132 ) ) ;
#9248 = CARTESIAN_POINT ( 'NONE',  ( 2.500000000000000000, 0.000000000000000000, -6.099999999999999645 ) ) ;
#9249 = CARTESIAN_POINT ( 'NONE',  ( -1.477628194636992243, 49.49121550494065502, -20.47411891050684218 ) ) ;
#9250 = CARTESIAN_POINT ( 'NONE',  ( -45.81092964171354964, 71.80742102382775727, -12.92463648794852205 ) ) ;
#9251 = ORIENTED_EDGE ( 'NONE', *, *, #8735, .F. ) ;
#9252 = CIRCLE ( 'NONE', #3140, 1.500000000000001332 ) ;
#9253 = CARTESIAN_POINT ( 'NONE',  ( -71.84375000204838102, 55.00000000000000000, -25.81189881249999729 ) ) ;
#9254 = CARTESIAN_POINT ( 'NONE',  ( -72.40625000409679046, 80.00000000000001421, 10.35533905932737397 ) ) ;
#9255 = FACE_OUTER_BOUND ( 'NONE', #1993, .T. ) ;
#9256 = VERTEX_POINT ( 'NONE', #10365 ) ;
#9257 = CARTESIAN_POINT ( 'NONE',  ( -37.85565285117030498, 44.43519602072407082, -18.33024205669471840 ) ) ;
#9258 = CARTESIAN_POINT ( 'NONE',  ( -55.45210586135002728, 71.88485191958531573, 12.52183031059725771 ) ) ;
#9259 = CARTESIAN_POINT ( 'NONE',  ( -78.00000000000001421, 67.72792206135787296, -4.242637315201482906 ) ) ;
#9260 = FACE_OUTER_BOUND ( 'NONE', #9681, .T. ) ;
#9261 = VERTEX_POINT ( 'NONE', #3296 ) ;
#9262 = CARTESIAN_POINT ( 'NONE',  ( -77.84375000000001421, 65.35533905932737753, 24.99999999999999645 ) ) ;
#9263 = CARTESIAN_POINT ( 'NONE',  ( -34.28557208676265589, 54.99469277422922175, -0.0007481125482429651277 ) ) ;
#9264 = CARTESIAN_POINT ( 'NONE',  ( -48.90475262238859244, 59.99999999999997158, -9.564595459368971197E-12 ) ) ;
#9265 = CARTESIAN_POINT ( 'NONE',  ( -78.00000000000001421, 63.48528137423857487, 3.371917795327861178E-06 ) ) ;
#9266 = DIRECTION ( 'NONE',  ( -1.000000000000000000, -0.000000000000000000, -0.000000000000000000 ) ) ;
#9267 = CARTESIAN_POINT ( 'NONE',  ( -54.92282199211652483, 67.36828978179006810, 6.609266281412864430 ) ) ;
#9268 = ORIENTED_EDGE ( 'NONE', *, *, #4299, .T. ) ;
#9269 = CARTESIAN_POINT ( 'NONE',  ( 0.8557374297261139962, 42.07536394375442512, -16.80742094040031631 ) ) ;
#9270 = DIRECTION ( 'NONE',  ( -1.000000000000000000, 0.000000000000000000, 0.000000000000000000 ) ) ;
#9271 = DIRECTION ( 'NONE',  ( 0.000000000000000000, 1.000000000000000000, 0.000000000000000000 ) ) ;
#9272 = CARTESIAN_POINT ( 'NONE',  ( -2.500000000000000000, 3.061616997868383141E-16, -3.832189483390572970 ) ) ;
#9273 = CARTESIAN_POINT ( 'NONE',  ( -11.01335487196557850, 69.13152664304863038, -20.62949354447422223 ) ) ;
#9274 = CARTESIAN_POINT ( 'NONE',  ( -78.50000000204840944, 44.30836144126053000, 25.81189881250000795 ) ) ;
#9275 = CIRCLE ( 'NONE', #1247, 3.000000000000000000 ) ;
#9276 = ORIENTED_EDGE ( 'NONE', *, *, #11718, .T. ) ;
#9277 = CARTESIAN_POINT ( 'NONE',  ( -78.78125000204839523, 73.25176868561975141, 18.25176868561974075 ) ) ;
#9278 = VERTEX_POINT ( 'NONE', #10535 ) ;
#9279 = CARTESIAN_POINT ( 'NONE',  ( -60.99710787470219486, 49.63646281896018309, 12.94522044443767683 ) ) ;
#9280 = ADVANCED_FACE ( 'NONE', ( #8812 ), #9469, .F. ) ;
#9281 = DIRECTION ( 'NONE',  ( -1.000000000000000000, -0.000000000000000000, -0.000000000000000000 ) ) ;
#9282 = CARTESIAN_POINT ( 'NONE',  ( -75.00000000000000000, 78.32225602221440397, 9.188098902483863739 ) ) ;
#9283 = DIRECTION ( 'NONE',  ( -9.813077866773612233E-16, 1.000000000000000000, 0.000000000000000000 ) ) ;
#9284 = ORIENTED_EDGE ( 'NONE', *, *, #5592, .T. ) ;
#9285 = VECTOR ( 'NONE', #2141, 1000.000000000000000 ) ;
#9286 = CARTESIAN_POINT ( 'NONE',  ( -74.65625000000008527, 44.64466094067429225, 25.00000000000147082 ) ) ;
#9287 = CARTESIAN_POINT ( 'NONE',  ( -76.62500000409677625, 55.00000000000000000, 24.99999999999999645 ) ) ;
#9288 = DIRECTION ( 'NONE',  ( -1.000000000000000000, -0.000000000000000000, -0.000000000000000000 ) ) ;
#9289 = LINE ( 'NONE', #8745, #7461 ) ;
#9290 = CARTESIAN_POINT ( 'NONE',  ( 19.44332440029096887, 58.51573196296779855, 6.093031587449661224 ) ) ;
#9291 = EDGE_CURVE ( 'NONE', #43, #1798, #10590, .T. ) ;
#9292 = CARTESIAN_POINT ( 'NONE',  ( -20.34731364127066655, 75.86048710458229039, 7.023288102819432055 ) ) ;
#9293 = CIRCLE ( 'NONE', #5107, 2.500000000000000000 ) ;
#9294 = EDGE_CURVE ( 'NONE', #896, #4200, #9502, .T. ) ;
#9295 = EDGE_CURVE ( 'NONE', #5363, #1831, #3375, .T. ) ;
#9296 = LINE ( 'NONE', #1089, #9689 ) ;
#9297 = ORIENTED_EDGE ( 'NONE', *, *, #11161, .T. ) ;
#9298 = CARTESIAN_POINT ( 'NONE',  ( 14.99999999999999289, 39.99999999999999289, 19.99999999999999289 ) ) ;
#9299 = DIRECTION ( 'NONE',  ( -1.000000000000000000, -0.000000000000000000, -0.000000000000000000 ) ) ;
#9300 = EDGE_LOOP ( 'NONE', ( #807, #2466, #7771, #4189 ) ) ;
#9301 = CARTESIAN_POINT ( 'NONE',  ( 2.881307801134362023, 34.60859193927083055, -5.107160905361891601 ) ) ;
#9302 = CARTESIAN_POINT ( 'NONE',  ( -71.93750000204838102, 65.69163855873948421, -25.81189881250000440 ) ) ;
#9303 = ADVANCED_FACE ( 'NONE', ( #7680 ), #10449, .F. ) ;
#9304 = ADVANCED_FACE ( 'NONE', ( #1255 ), #11429, .F. ) ;
#9305 = PRODUCT_DEFINITION_SHAPE ( 'NONE', 'NONE',  #4032 ) ;
#9306 = ADVANCED_FACE ( 'NONE', ( #2219, #8637 ), #418, .F. ) ;
#9307 = LINE ( 'NONE', #4761, #7504 ) ;
#9308 = CARTESIAN_POINT ( 'NONE',  ( -46.52239103091250172, 73.32882989972571863, -10.56393531560676102 ) ) ;
#9309 = VECTOR ( 'NONE', #3843, 1000.000000000000000 ) ;
#9310 = VECTOR ( 'NONE', #3052, 1000.000000000000114 ) ;
#9311 = CARTESIAN_POINT ( 'NONE',  ( -32.17314280228392676, 34.29902663375150240, -4.109485608336678197 ) ) ;
#9312 = VERTEX_POINT ( 'NONE', #4022 ) ;
#9313 = DIRECTION ( 'NONE',  ( 1.000000000000000000, 6.033820786006286457E-17, -0.000000000000000000 ) ) ;
#9314 = DIRECTION ( 'NONE',  ( -1.000000000000000000, -9.813077866773612233E-16, 0.000000000000000000 ) ) ;
#9315 = CARTESIAN_POINT ( 'NONE',  ( 2.881307801134362023, 34.60859193927083055, -5.107160905361891601 ) ) ;
#9316 = ORIENTED_EDGE ( 'NONE', *, *, #3645, .T. ) ;
#9317 = CARTESIAN_POINT ( 'NONE',  ( -37.14429486108867451, 42.07659820469130096, -16.80634109873993864 ) ) ;
#9318 = VECTOR ( 'NONE', #7605, 1000.000000000000000 ) ;
#9319 = CARTESIAN_POINT ( 'NONE',  ( -44.66281104389123868, 63.04473320575852568, -19.42304942373100829 ) ) ;
#9320 = CARTESIAN_POINT ( 'NONE',  ( -73.06250000409677625, 37.32233047033631124, -17.67766952966368166 ) ) ;
#9321 = PRESENTATION_LAYER_ASSIGNMENT (  '', '', ( #5128 ) ) ;
#9322 = DIRECTION ( 'NONE',  ( -1.000000000000000000, 0.000000000000000000, 0.000000000000000000 ) ) ;
#9323 = CARTESIAN_POINT ( 'NONE',  ( -78.00000000000001421, 54.99999999999998579, -8.485278002320759683 ) ) ;
#9324 = ORIENTED_EDGE ( 'NONE', *, *, #1191, .T. ) ;
#9325 = CARTESIAN_POINT ( 'NONE',  ( -75.87500000000000000, 30.00000000000000355, 4.592425496802573578E-15 ) ) ;
#9326 = CARTESIAN_POINT ( 'NONE',  ( -43.90973736884477319, 55.00080601838077143, -0.005934653685857244065 ) ) ;
#9327 = CARTESIAN_POINT ( 'NONE',  ( -40.35278372931369262, 55.66209291482490329, -4.999970240424343793 ) ) ;
#9328 = VECTOR ( 'NONE', #595, 1000.000000000000000 ) ;
#9329 = DIRECTION ( 'NONE',  ( 0.000000000000000000, 0.000000000000000000, -1.000000000000000000 ) ) ;
#9330 = CARTESIAN_POINT ( 'NONE',  ( -9.750467871106947015, 59.44169190721913765, -5.412448594069168450 ) ) ;
#9331 = VERTEX_POINT ( 'NONE', #9589 ) ;
#9332 = CARTESIAN_POINT ( 'NONE',  ( -2.188986190505546769, 52.25407376895000056, -20.97627476078892528 ) ) ;
#9333 = UNCERTAINTY_MEASURE_WITH_UNIT (LENGTH_MEASURE( 1.000000000000000082E-05 ), #2744, 'distance_accuracy_value', 'NONE');
#9334 = DIRECTION ( 'NONE',  ( 0.000000000000000000, 0.000000000000000000, 1.000000000000000000 ) ) ;
#9335 = DIRECTION ( 'NONE',  ( -0.000000000000000000, -0.000000000000000000, 1.000000000000000000 ) ) ;
#9336 = CARTESIAN_POINT ( 'NONE',  ( -80.00000000000001421, 63.48528137423857487, 3.371917795327861178E-06 ) ) ;
#9337 = CARTESIAN_POINT ( 'NONE',  ( -21.39751393901811838, 76.72268714209511131, -12.45540278537336754 ) ) ;
#9338 = CARTESIAN_POINT ( 'NONE',  ( -72.31250000204839523, 29.18810118750000626, -10.69163855873949309 ) ) ;
#9339 = AXIS2_PLACEMENT_3D ( 'NONE', #7972, #3532, #1732 ) ;
#9340 = ORIENTED_EDGE ( 'NONE', *, *, #4904, .F. ) ;
#9341 = CARTESIAN_POINT ( 'NONE',  ( -73.81250000204839523, 29.18810118750000981, 10.69163855873950020 ) ) ;
#9342 = ORIENTED_EDGE ( 'NONE', *, *, #7566, .F. ) ;
#9343 = CARTESIAN_POINT ( 'NONE',  ( 25.08633069608793420, 79.82547947451034531, 2.979094639268365263 ) ) ;
#9344 = CARTESIAN_POINT ( 'NONE',  ( 21.14436220910852882, 71.77416011014268804, 12.89076390558360075 ) ) ;
#9345 = DIRECTION ( 'NONE',  ( 1.000000000000000000, 0.000000000000000000, 0.000000000000000000 ) ) ;
#9346 = EDGE_CURVE ( 'NONE', #4386, #6519, #4924, .T. ) ;
#9347 = CARTESIAN_POINT ( 'NONE',  ( -75.00000000000000000, 79.90134559235561085, -4.530844741510550833 ) ) ;
#9348 = DIRECTION ( 'NONE',  ( 0.000000000000000000, 0.000000000000000000, 1.000000000000000000 ) ) ;
#9349 = VERTEX_POINT ( 'NONE', #356 ) ;
#9350 = CARTESIAN_POINT ( 'NONE',  ( -74.75000000000000000, 55.00000000000000000, 24.99999999999999645 ) ) ;
#9351 = CARTESIAN_POINT ( 'NONE',  ( -72.87500000409677625, 55.00000000000000000, -24.99999999999999645 ) ) ;
#9352 = AXIS2_PLACEMENT_3D ( 'NONE', #6105, #2438, #3217 ) ;
#9353 = DIRECTION ( 'NONE',  ( -6.033820786006286457E-17, 1.000000000000000000, 0.000000000000000000 ) ) ;
#9354 = PLANE ( 'NONE',  #2284 ) ;
#9355 = CARTESIAN_POINT ( 'NONE',  ( 15.55675285225959570, 54.08367678788073363, 7.025375982562417576 ) ) ;
#9356 = CARTESIAN_POINT ( 'NONE',  ( -2.500000000000000000, 3.061616997868383141E-16, -0.5394676594665810399 ) ) ;
#9357 = AXIS2_PLACEMENT_3D ( 'NONE', #5324, #2564, #1657 ) ;
#9358 = CYLINDRICAL_SURFACE ( 'NONE', #4715, 25.00000000000000355 ) ;
#9359 = ORIENTED_EDGE ( 'NONE', *, *, #1871, .F. ) ;
#9360 = DIRECTION ( 'NONE',  ( -1.000000000000000000, -0.000000000000000000, -0.000000000000000000 ) ) ;
#9361 = DIRECTION ( 'NONE',  ( -0.8191520442889974607, 0.000000000000000000, -0.5735764363510379438 ) ) ;
#9362 = ORIENTED_EDGE ( 'NONE', *, *, #10767, .F. ) ;
#9363 = CARTESIAN_POINT ( 'NONE',  ( -61.00490302436042356, 55.00059028654953153, 21.02810969917934614 ) ) ;
#9364 = CARTESIAN_POINT ( 'NONE',  ( -79.34375000204839523, 55.00000000000000000, -25.81189881249999729 ) ) ;
#9365 = DIRECTION ( 'NONE',  ( 0.000000000000000000, 0.000000000000000000, 1.000000000000000000 ) ) ;
#9366 = CARTESIAN_POINT ( 'NONE',  ( -61.32723930490969622, 46.95308112547827051, 19.41976192622660946 ) ) ;
#9367 = FILL_AREA_STYLE_COLOUR ( '', #8518 ) ;
#9368 = CARTESIAN_POINT ( 'NONE',  ( -78.00000000000002842, 46.51471862576140381, 3.371917798797308130E-06 ) ) ;
#9369 = ORIENTED_EDGE ( 'NONE', *, *, #1181, .T. ) ;
#9370 = FACE_OUTER_BOUND ( 'NONE', #9076, .T. ) ;
#9371 = EDGE_CURVE ( 'NONE', #5671, #1709, #6965, .T. ) ;
#9372 = CARTESIAN_POINT ( 'NONE',  ( -72.78125000409680467, 65.35533905932757648, -24.99999999999979039 ) ) ;
#9373 = VECTOR ( 'NONE', #3767, 1000.000000000000000 ) ;
#9374 = CARTESIAN_POINT ( 'NONE',  ( 22.99999999999999645, 76.00000000000000000, 0.000000000000000000 ) ) ;
#9375 = VERTEX_POINT ( 'NONE', #3236 ) ;
#9376 = CARTESIAN_POINT ( 'NONE',  ( -50.94162072875351299, 76.01658590998553677, 2.059423418002142459 ) ) ;
#9377 = CARTESIAN_POINT ( 'NONE',  ( -65.06671514604981610, 41.61929618219224380, 16.30332023460171698 ) ) ;
#9378 = CARTESIAN_POINT ( 'NONE',  ( -77.93750000409679046, 37.32233047033631124, 17.67766952966369232 ) ) ;
#9379 = AXIS2_PLACEMENT_3D ( 'NONE', #8494, #3936, #6588 ) ;
#9380 = DIRECTION ( 'NONE',  ( -1.000000000000000000, -0.000000000000000000, -0.000000000000000000 ) ) ;
#9381 = CARTESIAN_POINT ( 'NONE',  ( -75.31250000409677625, 72.67766952966368876, 17.67766952966368521 ) ) ;
#9382 = EDGE_CURVE ( 'NONE', #9830, #364, #8087, .T. ) ;
#9383 = EDGE_LOOP ( 'NONE', ( #3618, #6972 ) ) ;
#9384 = CARTESIAN_POINT ( 'NONE',  ( -77.65625000000001421, 44.64466094067262958, 25.00000000000001066 ) ) ;
#9385 = CARTESIAN_POINT ( 'NONE',  ( -74.99999999999997158, 57.62508896066697872, -25.69211664326230604 ) ) ;
#9386 = CARTESIAN_POINT ( 'NONE',  ( -80.00000000000001421, 67.72792206135787296, 12.72792543327562775 ) ) ;
#9387 = VECTOR ( 'NONE', #735, 1000.000000000000000 ) ;
#9388 = CARTESIAN_POINT ( 'NONE',  ( 53.00000000000000000, 51.46446609406726935, 3.535533905932731091 ) ) ;
#9389 = AXIS2_PLACEMENT_3D ( 'NONE', #11051, #2748, #1956 ) ;
#9390 = AXIS2_PLACEMENT_3D ( 'NONE', #429, #5966, #3911 ) ;
#9391 = FACE_OUTER_BOUND ( 'NONE', #7742, .T. ) ;
#9392 = CARTESIAN_POINT ( 'NONE',  ( -64.83840380677510495, 47.18714368648432611, 11.70375861309407206 ) ) ;
#9393 = ORIENTED_EDGE ( 'NONE', *, *, #9466, .T. ) ;
#9394 = CARTESIAN_POINT ( 'NONE',  ( 0.1442708919848544047, 44.43605983923426805, -18.32883121229183487 ) ) ;
#9395 = CARTESIAN_POINT ( 'NONE',  ( 0.000000000000000000, 0.000000000000000000, -5.210428571428570521 ) ) ;
#9396 = DIRECTION ( 'NONE',  ( -0.000000000000000000, -0.000000000000000000, 1.000000000000000000 ) ) ;
#9397 = DIRECTION ( 'NONE',  ( 0.000000000000000000, 1.000000000000000000, 0.000000000000000000 ) ) ;
#9398 = CARTESIAN_POINT ( 'NONE',  ( -25.28844287072157471, 79.99882686206473181, -0.8862795495640891641 ) ) ;
#9399 = CARTESIAN_POINT ( 'NONE',  ( -74.18750000204838102, 44.30836144126053000, 25.81189881250000795 ) ) ;
#9400 = ORIENTED_EDGE ( 'NONE', *, *, #1731, .F. ) ;
#9401 = CARTESIAN_POINT ( 'NONE',  ( -73.71875000204839523, 29.18810118750000271, 4.741568889096522788E-15 ) ) ;
#9402 = CIRCLE ( 'NONE', #7691, 21.50000000000000000 ) ;
#9403 = VERTEX_POINT ( 'NONE', #3179 ) ;
#9404 = CARTESIAN_POINT ( 'NONE',  ( 25.28926814670273515, 79.99953533380057991, 0.8669296567843869372 ) ) ;
#9405 = CARTESIAN_POINT ( 'NONE',  ( -41.74394153288059783, 59.06666331196394282, -13.40395870027933078 ) ) ;
#9406 = DIRECTION ( 'NONE',  ( -1.000000000000000000, 0.000000000000000000, 0.000000000000000000 ) ) ;
#9407 = ADVANCED_FACE ( 'NONE', ( #9644 ), #5047, .T. ) ;
#9408 = CARTESIAN_POINT ( 'NONE',  ( -75.00000000000001421, 75.69461608703821298, -15.00647013622189618 ) ) ;
#9409 = DIRECTION ( 'NONE',  ( -1.000000000000000000, 0.000000000000000000, 0.000000000000000000 ) ) ;
#9410 = VECTOR ( 'NONE', #4277, 1000.000000000000000 ) ;
#9411 = ORIENTED_EDGE ( 'NONE', *, *, #9071, .F. ) ;
#9412 = DIRECTION ( 'NONE',  ( -0.8191520442889913545, 0.000000000000000000, -0.5735764363510468256 ) ) ;
#9413 = CARTESIAN_POINT ( 'NONE',  ( -74.56250000409677625, 37.32233047033631124, -17.67766952966368166 ) ) ;
#9414 = CARTESIAN_POINT ( 'NONE',  ( -39.98517722295121501, 52.49184747003998552, -4.337707995793770976 ) ) ;
#9415 = EDGE_LOOP ( 'NONE', ( #11089, #2778, #2422, #9013 ) ) ;
#9416 = ADVANCED_BREP_SHAPE_REPRESENTATION ( '', ( #980, #4738 ), #4498 ) ;
#9417 = CARTESIAN_POINT ( 'NONE',  ( 8.750843404857064911, 48.25223522016324296, 2.051079653697085892 ) ) ;
#9418 = CARTESIAN_POINT ( 'NONE',  ( -0.7331957588256760028, 64.99605696851789105, 19.59792961213366880 ) ) ;
#9419 = CYLINDRICAL_SURFACE ( 'NONE', #1073, 2.999999999999999112 ) ;
#9420 = VERTEX_POINT ( 'NONE', #5104 ) ;
#9421 = EDGE_CURVE ( 'NONE', #3207, #3150, #8751, .T. ) ;
#9422 = CARTESIAN_POINT ( 'NONE',  ( 53.00000000000000000, 51.46446609406726935, 3.535533905932731091 ) ) ;
#9423 = DIRECTION ( 'NONE',  ( 0.000000000000000000, 1.000000000000000000, 0.000000000000000000 ) ) ;
#9424 = ORIENTED_EDGE ( 'NONE', *, *, #2586, .F. ) ;
#9425 = CARTESIAN_POINT ( 'NONE',  ( -29.49360042904642043, 37.45509264529403737, 11.71531283165970727 ) ) ;
#9426 = CARTESIAN_POINT ( 'NONE',  ( -72.12500000204840944, 29.18810118750000626, -10.69163855873949309 ) ) ;
#9427 = CARTESIAN_POINT ( 'NONE',  ( -1.625240267017640655E-20, 65.42943686846950868, 22.72062601704910634 ) ) ;
#9428 = CARTESIAN_POINT ( 'NONE',  ( -52.88146049032556562, 73.03766007303350705, 10.81102556547625149 ) ) ;
#9429 = SURFACE_STYLE_FILL_AREA ( #1280 ) ;
#9430 = DIRECTION ( 'NONE',  ( 0.000000000000000000, 1.000000000000000000, 0.000000000000000000 ) ) ;
#9431 = VERTEX_POINT ( 'NONE', #11486 ) ;
#9432 = CARTESIAN_POINT ( 'NONE',  ( 0.000000000000000000, 0.000000000000000000, -3.832189483390572970 ) ) ;
#9433 = EDGE_CURVE ( 'NONE', #2377, #1407, #9097, .T. ) ;
#9434 = CARTESIAN_POINT ( 'NONE',  ( -1.871122143093896906, 51.94779910732768258, -3.973801861892843235 ) ) ;
#9435 = CARTESIAN_POINT ( 'NONE',  ( -78.21875000000004263, 79.99999999999992895, -10.35533905932734910 ) ) ;
#9436 = VERTEX_POINT ( 'NONE', #762 ) ;
#9437 = CARTESIAN_POINT ( 'NONE',  ( 15.85562909902672679, 60.50729566700048423, 20.47119405379366697 ) ) ;
#9438 = CARTESIAN_POINT ( 'NONE',  ( 11.79372827400108470, 51.34087032111902715, 13.61835106791356154 ) ) ;
#9439 = CARTESIAN_POINT ( 'NONE',  ( -78.59375000000001421, 44.64466094067047663, -24.99999999999782219 ) ) ;
#9440 = DIRECTION ( 'NONE',  ( -1.000000000000000000, -0.000000000000000000, -0.000000000000000000 ) ) ;
#9441 = CARTESIAN_POINT ( 'NONE',  ( -15.09523335307150838, 60.00000000000000000, 4.640896189903090912E-12 ) ) ;
#9442 = CARTESIAN_POINT ( 'NONE',  ( -75.12500000000007105, 79.99999999999990052, -1.530808498934185013E-15 ) ) ;
#9443 = ADVANCED_FACE ( 'NONE', ( #9818, #1729 ), #8094, .T. ) ;
#9444 = ORIENTED_EDGE ( 'NONE', *, *, #48, .T. ) ;
#9445 = CARTESIAN_POINT ( 'NONE',  ( -15.00000000000000000, -30.00000000000000000, 10.00000000000000000 ) ) ;
#9446 = CARTESIAN_POINT ( 'NONE',  ( -79.34375000204839523, 55.00000000000000000, -25.81189881249999729 ) ) ;
#9447 =( REPRESENTATION_RELATIONSHIP ('NONE','NONE', #5489, #11597 ) REPRESENTATION_RELATIONSHIP_WITH_TRANSFORMATION ( #6327 )SHAPE_REPRESENTATION_RELATIONSHIP( ) );
#9448 = EDGE_CURVE ( 'NONE', #5671, #4962, #2577, .T. ) ;
#9449 = LINE ( 'NONE', #3759, #10921 ) ;
#9450 = ADVANCED_FACE ( 'NONE', ( #6300 ), #877, .F. ) ;
#9451 = CYLINDRICAL_SURFACE ( 'NONE', #125, 25.00000000000000355 ) ;
#9452 = CARTESIAN_POINT ( 'NONE',  ( -63.96363525012968410, 49.00358019864930981, 12.67571071499552282 ) ) ;
#9453 = ORIENTED_EDGE ( 'NONE', *, *, #18, .T. ) ;
#9454 = SHAPE_REPRESENTATION ( 'hex nut gradec_iso_ISO - 4034 - M6 - S', ( #4738 ), #10420 ) ;
#9455 = CARTESIAN_POINT ( 'NONE',  ( -41.21475901749523274, 58.08538884819615333, -20.80179922188357011 ) ) ;
#9456 = DIRECTION ( 'NONE',  ( -0.000000000000000000, -0.000000000000000000, -1.000000000000000000 ) ) ;
#9457 = CARTESIAN_POINT ( 'NONE',  ( 39.99999999999999289, 55.00000000000000000, 0.000000000000000000 ) ) ;
#9458 = DIRECTION ( 'NONE',  ( -0.000000000000000000, -0.000000000000000000, -1.000000000000000000 ) ) ;
#9459 = CARTESIAN_POINT ( 'NONE',  ( -25.27843518572107229, 79.99023359000550215, 0.8195747360922619462 ) ) ;
#9460 = CARTESIAN_POINT ( 'NONE',  ( -72.40625000204838102, 29.18810118750000271, 4.741568889096522788E-15 ) ) ;
#9461 = EDGE_CURVE ( 'NONE', #2759, #7749, #4793, .T. ) ;
#9462 = VERTEX_POINT ( 'NONE', #10645 ) ;
#9463 = CARTESIAN_POINT ( 'NONE',  ( -71.56250000204838102, 80.81189881250001861, -10.69163855873949132 ) ) ;
#9464 = ORIENTED_EDGE ( 'NONE', *, *, #5592, .F. ) ;
#9465 = CARTESIAN_POINT ( 'NONE',  ( 5.841383071459858023, 66.54671248543735373, -22.17569923478663796 ) ) ;
#9466 = EDGE_CURVE ( 'NONE', #9124, #10874, #4347, .T. ) ;
#9467 = CARTESIAN_POINT ( 'NONE',  ( -59.54425338440577775, 52.94308673282063182, 13.86869692379441510 ) ) ;
#9468 = DIRECTION ( 'NONE',  ( -0.000000000000000000, -0.000000000000000000, -1.000000000000000000 ) ) ;
#9469 = CYLINDRICAL_SURFACE ( 'NONE', #1839, 1.500000000000000000 ) ;
#9470 = CARTESIAN_POINT ( 'NONE',  ( 5.000000000000000000, 2.886751345948124214, -6.099999999999999645 ) ) ;
#9471 = PRODUCT_DEFINITION_FORMATION_WITH_SPECIFIED_SOURCE ( 'ANY', '', #7403, .NOT_KNOWN. ) ;
#9472 = VERTEX_POINT ( 'NONE', #4378 ) ;
#9473 = CARTESIAN_POINT ( 'NONE',  ( -75.21875000000000000, 80.00000000000001421, -10.35533905932737753 ) ) ;
#9474 = CARTESIAN_POINT ( 'NONE',  ( -74.84375000409679046, 30.00000000000001421, 10.35533905932739174 ) ) ;
#9475 = CARTESIAN_POINT ( 'NONE',  ( -47.37975114575861824, 58.30660270781542920, -3.764775390512491438 ) ) ;
#9476 = EDGE_LOOP ( 'NONE', ( #1740, #9090, #3202, #9276 ) ) ;
#9477 = CARTESIAN_POINT ( 'NONE',  ( -20.41758684020055981, 55.68721290480836217, 6.980984518528451588 ) ) ;
#9478 = AXIS2_PLACEMENT_3D ( 'NONE', #7418, #2796, #6462 ) ;
#9479 = CARTESIAN_POINT ( 'NONE',  ( -73.15625000000008527, 44.64466094067268642, 24.99999999999986144 ) ) ;
#9480 = LINE ( 'NONE', #6622, #6439 ) ;
#9481 = ORIENTED_EDGE ( 'NONE', *, *, #7688, .T. ) ;
#9482 = DIRECTION ( 'NONE',  ( -6.033820786006286457E-17, 1.000000000000000000, 0.000000000000000000 ) ) ;
#9483 = CARTESIAN_POINT ( 'NONE',  ( -76.90625000204838102, 29.18810118750000271, 4.741568889096522788E-15 ) ) ;
#9484 = VERTEX_POINT ( 'NONE', #8031 ) ;
#9485 = CARTESIAN_POINT ( 'NONE',  ( -40.60828084101493829, 48.86090744392433294, -20.20262880343927847 ) ) ;
#9486 = CARTESIAN_POINT ( 'NONE',  ( -73.71875000204839523, 29.18810118750000271, 4.741568889096522788E-15 ) ) ;
#9487 = AXIS2_PLACEMENT_3D ( 'NONE', #9551, #5849, #5010 ) ;
#9488 = CARTESIAN_POINT ( 'NONE',  ( 47.00000000000000000, 51.46446609406726935, 3.535533905932731091 ) ) ;
#9489 = CARTESIAN_POINT ( 'NONE',  ( -70.34104699118840642, 33.99562393659799397, 0.006612473344882377653 ) ) ;
#9490 = DIRECTION ( 'NONE',  ( 0.000000000000000000, 1.000000000000000000, 0.000000000000000000 ) ) ;
#9491 = AXIS2_PLACEMENT_3D ( 'NONE', #4839, #10983, #2853 ) ;
#9492 = VERTEX_POINT ( 'NONE', #11668 ) ;
#9493 = CARTESIAN_POINT ( 'NONE',  ( 1.034159948410326981E-15, 5.773502691896260863, -6.099999999999999645 ) ) ;
#9494 = LINE ( 'NONE', #9557, #9931 ) ;
#9495 = EDGE_CURVE ( 'NONE', #8038, #30, #5865, .T. ) ;
#9496 = CARTESIAN_POINT ( 'NONE',  ( -44.07074648197151845, 61.10275710191199749, -20.11236068975357938 ) ) ;
#9497 = ORIENTED_EDGE ( 'NONE', *, *, #5169, .F. ) ;
#9498 = CARTESIAN_POINT ( 'NONE',  ( 4.403976020759948540, 34.06825102507477965, -2.059153462500010967 ) ) ;
#9499 = CARTESIAN_POINT ( 'NONE',  ( 2.544693516836439073, 41.40683613508774386, -3.404232400632562161 ) ) ;
#9500 = FACE_OUTER_BOUND ( 'NONE', #10701, .T. ) ;
#9501 = LINE ( 'NONE', #8548, #6239 ) ;
#9502 = CIRCLE ( 'NONE', #8935, 24.99999999999999645 ) ;
#9503 = LINE ( 'NONE', #2072, #11076 ) ;
#9504 = ORIENTED_EDGE ( 'NONE', *, *, #2939, .T. ) ;
#9505 = CARTESIAN_POINT ( 'NONE',  ( -79.15625000000000000, 44.64466094067262958, 25.00000000000001066 ) ) ;
#9506 = DIRECTION ( 'NONE',  ( -1.000000000000000000, -0.000000000000000000, -0.000000000000000000 ) ) ;
#9507 = EDGE_CURVE ( 'NONE', #3587, #10459, #11793, .T. ) ;
#9508 = DIRECTION ( 'NONE',  ( 0.000000000000000000, 0.000000000000000000, -1.000000000000000000 ) ) ;
#9509 = VECTOR ( 'NONE', #5604, 1000.000000000000000 ) ;
#9510 = DIRECTION ( 'NONE',  ( -1.000000000000000000, -0.000000000000000000, -0.000000000000000000 ) ) ;
#9511 = CARTESIAN_POINT ( 'NONE',  ( -28.22334563455873635, 50.71039758802199771, 5.585597018820382509 ) ) ;
#9512 = AXIS2_PLACEMENT_3D ( 'NONE', #1967, #5637, #7499 ) ;
#9513 = ORIENTED_EDGE ( 'NONE', *, *, #10019, .T. ) ;
#9514 = CARTESIAN_POINT ( 'NONE',  ( -53.45210586504737904, 71.88419113761085555, 12.52116934359859002 ) ) ;
#9515 = FACE_OUTER_BOUND ( 'NONE', #7209, .T. ) ;
#9516 = LINE ( 'NONE', #7729, #10399 ) ;
#9517 = CARTESIAN_POINT ( 'NONE',  ( -76.15625000204839523, 73.25176868561975141, -18.25176868561974430 ) ) ;
#9518 = PRODUCT_RELATED_PRODUCT_CATEGORY ( 'part', '', ( #2038 ) ) ;
#9519 = CARTESIAN_POINT ( 'NONE',  ( -76.25000000000000000, 55.00000000000000000, 24.99999999999999645 ) ) ;
#9520 = CARTESIAN_POINT ( 'NONE',  ( -74.65625000204838102, 80.81189881250000440, -1.580522963032174394E-15 ) ) ;
#9521 = VERTEX_POINT ( 'NONE', #939 ) ;
#9522 = CIRCLE ( 'NONE', #11612, 1.500000000000001332 ) ;
#9523 = CARTESIAN_POINT ( 'NONE',  ( -71.65625000204839523, 73.25176868561975141, -18.25176868561974430 ) ) ;
#9524 = FACE_BOUND ( 'NONE', #1046, .T. ) ;
#9525 = SURFACE_SIDE_STYLE ('',( #2553 ) ) ;
#9526 = MECHANICAL_DESIGN_GEOMETRIC_PRESENTATION_REPRESENTATION (  '', ( #5128 ), #11803 ) ;
#9527 = CARTESIAN_POINT ( 'NONE',  ( 4.881307793505825110, 34.60946683332392126, -5.106800360247272685 ) ) ;
#9528 = CARTESIAN_POINT ( 'NONE',  ( -71.40552368722833876, 77.35376350879521112, 12.90594348738575903 ) ) ;
#9529 = DIRECTION ( 'NONE',  ( -1.000000000000000000, 0.000000000000000000, 0.000000000000000000 ) ) ;
#9530 = ADVANCED_FACE ( 'NONE', ( #4785 ), #10641, .F. ) ;
#9531 = CARTESIAN_POINT ( 'NONE',  ( -78.00000000000002842, 42.27207793864211283, -5.742637315201479353 ) ) ;
#9532 = AXIS2_PLACEMENT_3D ( 'NONE', #8096, #10044, #8990 ) ;
#9533 = ORIENTED_EDGE ( 'NONE', *, *, #7659, .T. ) ;
#9534 = CARTESIAN_POINT ( 'NONE',  ( -72.59375000000000000, 44.64466094067260826, -24.99999999999998934 ) ) ;
#9535 = CARTESIAN_POINT ( 'NONE',  ( -71.75000000409677625, 30.00000000000000355, 4.592425496802573578E-15 ) ) ;
#9536 = CARTESIAN_POINT ( 'NONE',  ( -45.81573735730770380, 57.21589932804895540, -4.494086191879637759 ) ) ;
#9537 = ADVANCED_FACE ( 'NONE', ( #3762, #1840, #6474 ), #10286, .F. ) ;
#9538 = VERTEX_POINT ( 'NONE', #5629 ) ;
#9539 = EDGE_CURVE ( 'NONE', #7152, #11420, #3193, .T. ) ;
#9540 = CARTESIAN_POINT ( 'NONE',  ( 5.541412553157611498, 48.20653848766852434, -1.700702987377777253 ) ) ;
#9541 = DIRECTION ( 'NONE',  ( 1.000000000000000000, 0.000000000000000000, 0.000000000000000000 ) ) ;
#9542 = DIRECTION ( 'NONE',  ( 0.000000000000000000, 0.000000000000000000, 1.000000000000000000 ) ) ;
#9543 = ORIENTED_EDGE ( 'NONE', *, *, #4024, .F. ) ;
#9544 = CARTESIAN_POINT ( 'NONE',  ( 19.13861104931596202, 74.87002429251506896, 9.536576732248796873 ) ) ;
#9545 = CARTESIAN_POINT ( 'NONE',  ( -79.34375000204839523, 73.25176868561975141, -18.25176868561974430 ) ) ;
#9546 = AXIS2_PLACEMENT_3D ( 'NONE', #8076, #7353, #10026 ) ;
#9547 = ORIENTED_EDGE ( 'NONE', *, *, #3572, .F. ) ;
#9548 = CARTESIAN_POINT ( 'NONE',  ( -52.27495405780593529, 76.01412898031726684, 2.059423305703688811 ) ) ;
#9549 = CARTESIAN_POINT ( 'NONE',  ( -75.68750000204839523, 65.69163855873949842, 25.81189881250000440 ) ) ;
#9550 = CARTESIAN_POINT ( 'NONE',  ( -75.21875000409676204, 65.35533905932724963, 25.00000000000012434 ) ) ;
#9551 = CARTESIAN_POINT ( 'NONE',  ( -78.00000000000002842, 50.75735931288069480, 4.242644059037076865 ) ) ;
#9552 = SURFACE_STYLE_FILL_AREA ( #1405 ) ;
#9553 = AXIS2_PLACEMENT_3D ( 'NONE', #1473, #5988, #6941 ) ;
#9554 = CYLINDRICAL_SURFACE ( 'NONE', #8543, 2.500000000000000000 ) ;
#9555 = ORIENTED_EDGE ( 'NONE', *, *, #11787, .F. ) ;
#9556 = FACE_OUTER_BOUND ( 'NONE', #1539, .T. ) ;
#9557 = CARTESIAN_POINT ( 'NONE',  ( -78.00000000000001421, 67.72792206135787296, -11.22791868944004534 ) ) ;
#9558 = CARTESIAN_POINT ( 'NONE',  ( -34.17314261869798742, 34.29999169977881479, -4.109493429249395646 ) ) ;
#9559 = EDGE_LOOP ( 'NONE', ( #6371, #11255, #2410, #3232 ) ) ;
#9560 = CARTESIAN_POINT ( 'NONE',  ( -0.4775959007562765590, 42.07767894935109609, -16.80510553145697727 ) ) ;
#9561 = AXIS2_PLACEMENT_3D ( 'NONE', #2798, #5622, #87 ) ;
#9562 = CARTESIAN_POINT ( 'NONE',  ( -13.87290721739879551, 68.98200347986859526, -1.830994221428368540 ) ) ;
#9563 = PLANE ( 'NONE',  #9553 ) ;
#9564 = FACE_OUTER_BOUND ( 'NONE', #3858, .T. ) ;
#9565 = AXIS2_PLACEMENT_3D ( 'NONE', #813, #8086, #7307 ) ;
#9566 = FACE_OUTER_BOUND ( 'NONE', #4579, .T. ) ;
#9567 = ORIENTED_EDGE ( 'NONE', *, *, #2655, .T. ) ;
#9568 = CARTESIAN_POINT ( 'NONE',  ( -74.46875000000000000, 30.00000000000001421, 10.35533905932739174 ) ) ;
#9569 = LINE ( 'NONE', #8675, #7017 ) ;
#9570 = DIRECTION ( 'NONE',  ( 0.000000000000000000, -1.000000000000000000, 0.000000000000000000 ) ) ;
#9571 = CARTESIAN_POINT ( 'NONE',  ( 14.99999999999999645, 5.000000000000000000, 30.00000000000000711 ) ) ;
#9572 = CARTESIAN_POINT ( 'NONE',  ( -20.24961059810222963, 59.45058868119262740, 5.422033872742003879 ) ) ;
#9573 = VERTEX_POINT ( 'NONE', #2806 ) ;
#9574 = CARTESIAN_POINT ( 'NONE',  ( -29.26269115883859939, 34.87241548204915631, 6.108265559058850158 ) ) ;
#9575 = ADVANCED_FACE ( 'NONE', ( #8377, #157 ), #6410, .F. ) ;
#9576 = CARTESIAN_POINT ( 'NONE',  ( 39.99999999999999289, 39.99999999999999289, 19.99999999999999289 ) ) ;
#9577 = CARTESIAN_POINT ( 'NONE',  ( 0.000000000000000000, 0.000000000000000000, -25.03750572909317285 ) ) ;
#9578 = CARTESIAN_POINT ( 'NONE',  ( -74.75000000204839523, 65.69163855873948421, -25.81189881250000084 ) ) ;
#9579 = CARTESIAN_POINT ( 'NONE',  ( -23.35334274943035737, 78.35318589264019806, 8.957355889116216829 ) ) ;
#9580 = DIRECTION ( 'NONE',  ( 1.000000000000000000, 6.033820786006286457E-17, -0.000000000000000000 ) ) ;
#9581 = ORIENTED_EDGE ( 'NONE', *, *, #6453, .F. ) ;
#9582 = ADVANCED_FACE ( 'NONE', ( #5567 ), #3761, .T. ) ;
#9583 = CARTESIAN_POINT ( 'NONE',  ( -72.50000000204839523, 44.30836144126053000, 25.81189881250000795 ) ) ;
#9584 = FACE_BOUND ( 'NONE', #9137, .T. ) ;
#9585 = ORIENTED_EDGE ( 'NONE', *, *, #1460, .T. ) ;
#9586 = CARTESIAN_POINT ( 'NONE',  ( -26.94161418247137263, 38.68192823000178038, 13.40559829713685502 ) ) ;
#9587 = CIRCLE ( 'NONE', #401, 29.00000000000000355 ) ;
#9588 = FACE_OUTER_BOUND ( 'NONE', #11183, .T. ) ;
#9589 = CARTESIAN_POINT ( 'NONE',  ( -78.00000000000001421, 67.72792206135787296, 2.742644059037073312 ) ) ;
#9590 = LINE ( 'NONE', #5952, #7624 ) ;
#9591 = ORIENTED_EDGE ( 'NONE', *, *, #64, .T. ) ;
#9592 = CYLINDRICAL_SURFACE ( 'NONE', #6358, 4.999999999999997335 ) ;
#9593 = CIRCLE ( 'NONE', #8068, 1.500000000000001332 ) ;
#9594 = VECTOR ( 'NONE', #367, 1000.000000000000000 ) ;
#9595 = CARTESIAN_POINT ( 'NONE',  ( -76.06250000000000000, 37.32233047033631124, 17.67766952966369232 ) ) ;
#9596 = CARTESIAN_POINT ( 'NONE',  ( -2.500000000000000000, 3.061616997868383141E-16, -1.403639088038009630 ) ) ;
#9597 = CYLINDRICAL_SURFACE ( 'NONE', #6159, 1.500000000000000000 ) ;
#9598 = ORIENTED_EDGE ( 'NONE', *, *, #349, .T. ) ;
#9599 = EDGE_CURVE ( 'NONE', #5447, #3221, #9879, .T. ) ;
#9600 =( BOUNDED_CURVE ( )  B_SPLINE_CURVE ( 2, ( #3038, #2358, #6525, #10277, #9442, #6029, #1231 ),
 .UNSPECIFIED., .F., .T. ) 
 B_SPLINE_CURVE_WITH_KNOTS ( ( 3, 2, 2, 3 ),
 ( 0.4753074076739236542, 0.4951195077574221948, 0.5149316078409206243, 0.5280270264772872757 ),
 .UNSPECIFIED. ) 
 CURVE ( )  GEOMETRIC_REPRESENTATION_ITEM ( )  RATIONAL_B_SPLINE_CURVE ( ( 0.9999999999998887557, 0.9238795325113978718, 0.9999999999999998890, 0.9238795325112867385, 0.9999999999999998890, 0.9496858291468608382, 0.9658850645340137930 ) ) 
 REPRESENTATION_ITEM ( '' )  );
#9601 = CARTESIAN_POINT ( 'NONE',  ( -27.70870029355219089, 48.67231285529162932, 2.993251960717111082 ) ) ;
#9602 = CARTESIAN_POINT ( 'NONE',  ( -6.995124206613962947, 66.69163081399298676, 18.63899971507076003 ) ) ;
#9603 = CIRCLE ( 'NONE', #9820, 2.500000000000000000 ) ;
#9604 = DIRECTION ( 'NONE',  ( -1.000000000000000000, -0.000000000000000000, -0.000000000000000000 ) ) ;
#9605 = CIRCLE ( 'NONE', #599, 5.000000000000000888 ) ;
#9606 = ORIENTED_EDGE ( 'NONE', *, *, #3224, .F. ) ;
#9607 = CARTESIAN_POINT ( 'NONE',  ( 12.88440744682079497, 70.13069922856422522, -15.99938705239769021 ) ) ;
#9608 = CARTESIAN_POINT ( 'NONE',  ( -77.09375000204839523, 36.74823131438026280, 18.25176868561974786 ) ) ;
#9609 = ORIENTED_EDGE ( 'NONE', *, *, #6744, .T. ) ;
#9610 = CARTESIAN_POINT ( 'NONE',  ( -72.87500000204840944, 80.81189881250001861, 10.69163855873948599 ) ) ;
#9611 = DIRECTION ( 'NONE',  ( 1.000000000000000000, 0.000000000000000000, 0.000000000000000000 ) ) ;
#9612 = CARTESIAN_POINT ( 'NONE',  ( 1.907306313148354304, 54.98265195905499780, -0.01969434134204536141 ) ) ;
#9613 = DIRECTION ( 'NONE',  ( 0.8191520442889885789, 0.000000000000000000, 0.5735764363510507113 ) ) ;
#9614 = EDGE_CURVE ( 'NONE', #911, #4578, #3384, .T. ) ;
#9615 = ORIENTED_EDGE ( 'NONE', *, *, #11568, .T. ) ;
#9616 = DIRECTION ( 'NONE',  ( 0.000000000000000000, 0.000000000000000000, -1.000000000000000000 ) ) ;
#9617 = CARTESIAN_POINT ( 'NONE',  ( -44.66281104389123868, 63.04473320575852568, -19.42304942373100829 ) ) ;
#9618 = ORIENTED_EDGE ( 'NONE', *, *, #5113, .F. ) ;
#9619 = CARTESIAN_POINT ( 'NONE',  ( -12.14426256746178368, 75.47105121598427502, -5.507632465234872043 ) ) ;
#9620 = CARTESIAN_POINT ( 'NONE',  ( -20.78863981635950609, 62.20466253127742817, 12.01897416180004896 ) ) ;
#9621 = CARTESIAN_POINT ( 'NONE',  ( -78.00000000000002842, 59.24264068711927678, 12.72792543327563131 ) ) ;
#9622 = DIRECTION ( 'NONE',  ( -1.000000000000000000, -0.000000000000000000, -0.000000000000000000 ) ) ;
#9623 = CARTESIAN_POINT ( 'NONE',  ( -79.43750000204838102, 55.00000000000000000, -25.81189881249999729 ) ) ;
#9624 = ORIENTED_EDGE ( 'NONE', *, *, #6177, .F. ) ;
#9625 = CARTESIAN_POINT ( 'NONE',  ( -72.59375000000000000, 44.64466094067260826, -24.99999999999998934 ) ) ;
#9626 = CARTESIAN_POINT ( 'NONE',  ( -80.00000000000001421, 59.24264068711927678, -4.242637315201482906 ) ) ;
#9627 = DIRECTION ( 'NONE',  ( -1.000000000000000000, -0.000000000000000000, -0.000000000000000000 ) ) ;
#9628 = DIRECTION ( 'NONE',  ( -1.000000000000000000, 0.000000000000000000, 0.000000000000000000 ) ) ;
#9629 = CARTESIAN_POINT ( 'NONE',  ( -47.08425347821636819, 59.45470633346049993, -5.426572237033094659 ) ) ;
#9630 = ORIENTED_EDGE ( 'NONE', *, *, #7835, .T. ) ;
#9631 = CARTESIAN_POINT ( 'NONE',  ( -17.00387655282055377, 69.86881140706658755, 14.86941770366936311 ) ) ;
#9632 = CARTESIAN_POINT ( 'NONE',  ( 15.18896243380506306, 60.50666922109576262, 20.46968130491651650 ) ) ;
#9633 = LINE ( 'NONE', #579, #58 ) ;
#9634 = CARTESIAN_POINT ( 'NONE',  ( -77.37500000204838102, 80.81189881250000440, 10.69163855873948243 ) ) ;
#9635 = CARTESIAN_POINT ( 'NONE',  ( -18.44673231479036701, 74.35351539244358321, 15.87705593169374474 ) ) ;
#9636 = CARTESIAN_POINT ( 'NONE',  ( -75.68750000204839523, 65.69163855873949842, 25.81189881250000440 ) ) ;
#9637 = EDGE_LOOP ( 'NONE', ( #4693, #11626, #7558, #7229 ) ) ;
#9638 = CARTESIAN_POINT ( 'NONE',  ( -74.46875000409679046, 44.64466094067260826, -24.99999999999998934 ) ) ;
#9639 = FACE_BOUND ( 'NONE', #4264, .T. ) ;
#9640 = ORIENTED_EDGE ( 'NONE', *, *, #2510, .F. ) ;
#9641 = CARTESIAN_POINT ( 'NONE',  ( 0.8557374297261139962, 42.07536394375442512, -16.80742094040031631 ) ) ;
#9642 = CYLINDRICAL_SURFACE ( 'NONE', #1170, 4.999999999999984013 ) ;
#9643 = AXIS2_PLACEMENT_3D ( 'NONE', #9577, #9396, #4855 ) ;
#9644 = FACE_OUTER_BOUND ( 'NONE', #5304, .T. ) ;
#9645 = EDGE_CURVE ( 'NONE', #2363, #11604, #3703, .T. ) ;
#9646 = CARTESIAN_POINT ( 'NONE',  ( -80.00000000000001421, 59.24264068711927678, 5.742644059037073312 ) ) ;
#9647 = ORIENTED_EDGE ( 'NONE', *, *, #9291, .T. ) ;
#9648 = CARTESIAN_POINT ( 'NONE',  ( 3.556264818047235821, 3.720292241887088736, -6.018341802876231661 ) ) ;
#9649 = CARTESIAN_POINT ( 'NONE',  ( -73.81250000000000000, 72.67766952966368876, -17.67766952966368876 ) ) ;
#9650 = CARTESIAN_POINT ( 'NONE',  ( 2.500000000000003109, -4.330127018922193649, 0.000000000000000000 ) ) ;
#9651 = CARTESIAN_POINT ( 'NONE',  ( -80.00000000000001421, 46.51471862576140381, -9.985278002320759683 ) ) ;
#9652 = VERTEX_POINT ( 'NONE', #7548 ) ;
#9653 = ADVANCED_FACE ( 'NONE', ( #9391 ), #4928, .F. ) ;
#9654 = CARTESIAN_POINT ( 'NONE',  ( -35.77658090492886345, 50.68024773144422568, -5.615629700006128822 ) ) ;
#9655 = DIRECTION ( 'NONE',  ( -1.000000000000000000, 0.000000000000000000, 0.000000000000000000 ) ) ;
#9656 = DIRECTION ( 'NONE',  ( 0.000000000000000000, 1.000000000000000000, 0.000000000000000000 ) ) ;
#9657 = ORIENTED_EDGE ( 'NONE', *, *, #3310, .F. ) ;
#9658 = CARTESIAN_POINT ( 'NONE',  ( 21.03248180003672729, 76.42892261394429454, -5.031022656301434637 ) ) ;
#9659 = CARTESIAN_POINT ( 'NONE',  ( -78.68750000204838102, 44.30836144126052289, 25.81189881250000795 ) ) ;
#9660 = EDGE_LOOP ( 'NONE', ( #1767, #3485, #4823, #6500 ) ) ;
#9661 = CARTESIAN_POINT ( 'NONE',  ( -76.25000000204838102, 65.69163855873948421, -25.81189881250000440 ) ) ;
#9662 = DIRECTION ( 'NONE',  ( -1.000000000000000000, -0.000000000000000000, -0.000000000000000000 ) ) ;
#9663 = MECHANICAL_DESIGN_GEOMETRIC_PRESENTATION_REPRESENTATION (  '', ( #9094 ), #478 ) ;
#9664 = EDGE_CURVE ( 'NONE', #7121, #8651, #5691, .T. ) ;
#9665 = PLANE ( 'NONE',  #6747 ) ;
#9666 = CARTESIAN_POINT ( 'NONE',  ( -16.57640557450304897, 55.00618966384792685, 0.007491359115028465437 ) ) ;
#9667 = CARTESIAN_POINT ( 'NONE',  ( 0.000000000000000000, 0.000000000000000000, 0.000000000000000000 ) ) ;
#9668 = CARTESIAN_POINT ( 'NONE',  ( -75.00000000000000000, 31.54307055854626540, -10.27649223703322612 ) ) ;
#9669 = VERTEX_POINT ( 'NONE', #11116 ) ;
#9670 = CARTESIAN_POINT ( 'NONE',  ( 53.00000000000000000, 51.46446609406726935, 3.535533905932731091 ) ) ;
#9671 = EDGE_CURVE ( 'NONE', #9742, #4746, #11508, .T. ) ;
#9672 = CARTESIAN_POINT ( 'NONE',  ( -42.92935705524211443, 57.05913440163546113, -20.93112575922673102 ) ) ;
#9673 = EDGE_CURVE ( 'NONE', #301, #9224, #10942, .T. ) ;
#9674 = ORIENTED_EDGE ( 'NONE', *, *, #9421, .T. ) ;
#9675 = CARTESIAN_POINT ( 'NONE',  ( -7.262690645865875538, 64.91264328142536044, -18.55041054278238022 ) ) ;
#9676 = CARTESIAN_POINT ( 'NONE',  ( -0.07137196575059991110, 44.13905398550945591, -8.918958607883686440 ) ) ;
#9677 = CARTESIAN_POINT ( 'NONE',  ( -79.06250000000002842, 37.32233047033633966, 17.67766952966367100 ) ) ;
#9678 = CIRCLE ( 'NONE', #8340, 1.500000000000001332 ) ;
#9679 = EDGE_CURVE ( 'NONE', #6194, #9256, #1423, .T. ) ;
#9680 = CARTESIAN_POINT ( 'NONE',  ( -23.64880231868481175, 55.66116299125641831, 5.000007605738006511 ) ) ;
#9681 = EDGE_LOOP ( 'NONE', ( #5756, #5739, #3746, #2703 ) ) ;
#9682 = CARTESIAN_POINT ( 'NONE',  ( -74.09375000000000000, 44.64466094067260826, -24.99999999999998934 ) ) ;
#9683 = CARTESIAN_POINT ( 'NONE',  ( 21.85574933723554736, 73.37275400661043534, 10.58193396047185075 ) ) ;
#9684 = AXIS2_PLACEMENT_3D ( 'NONE', #5362, #9723, #4281 ) ;
#9685 = CARTESIAN_POINT ( 'NONE',  ( -78.00000000000001421, 59.24264068711927678, -5.742637315201482906 ) ) ;
#9686 = CARTESIAN_POINT ( 'NONE',  ( -27.44324756452158098, 51.46806551970854571, 6.132376716174161579 ) ) ;
#9687 = ORIENTED_EDGE ( 'NONE', *, *, #11176, .F. ) ;
#9688 = CARTESIAN_POINT ( 'NONE',  ( -40.92935782463053584, 57.05919160630219977, -20.93299540428984429 ) ) ;
#9689 = VECTOR ( 'NONE', #8406, 1000.000000000000000 ) ;
#9690 = CARTESIAN_POINT ( 'NONE',  ( -2.500000000000000000, 3.061616997868383141E-16, -0.3755037691048591086 ) ) ;
#9691 = DIRECTION ( 'NONE',  ( 0.000000000000000000, 1.000000000000000000, 0.000000000000000000 ) ) ;
#9692 = CARTESIAN_POINT ( 'NONE',  ( -76.25000000204838102, 65.69163855873948421, -25.81189881250000084 ) ) ;
#9693 = DIRECTION ( 'NONE',  ( 1.000000000000000000, 0.000000000000000000, 0.000000000000000000 ) ) ;
#9694 = CARTESIAN_POINT ( 'NONE',  ( -75.40625000204839523, 36.74823131438026280, 18.25176868561974786 ) ) ;
#9695 = ORIENTED_EDGE ( 'NONE', *, *, #18, .F. ) ;
#9696 = CARTESIAN_POINT ( 'NONE',  ( -73.71875000409677625, 65.35533905932737753, 24.99999999999999645 ) ) ;
#9697 = CYLINDRICAL_SURFACE ( 'NONE', #8987, 3.000000000000000888 ) ;
#9698 = FACE_BOUND ( 'NONE', #1393, .T. ) ;
#9699 = CARTESIAN_POINT ( 'NONE',  ( -28.67054321954914542, 35.57240153874681710, 8.046710727719679213 ) ) ;
#9700 = VECTOR ( 'NONE', #777, 1000.000000000000000 ) ;
#9701 = CARTESIAN_POINT ( 'NONE',  ( -78.00000000000002842, 50.75735931288069480, 4.242644059037076865 ) ) ;
#9702 = CARTESIAN_POINT ( 'NONE',  ( -75.00000000000000000, 76.68791387293471473, 12.43520775219157315 ) ) ;
#9703 = DIRECTION ( 'NONE',  ( 1.000000000000000000, 0.000000000000000000, 0.000000000000000000 ) ) ;
#9704 = CARTESIAN_POINT ( 'NONE',  ( -78.00000000000002842, 42.27207793864211283, -4.242637315201479353 ) ) ;
#9705 = AXIS2_PLACEMENT_3D ( 'NONE', #9029, #8287, #7127 ) ;
#9706 = CARTESIAN_POINT ( 'NONE',  ( -74.00000000000000000, 55.00000000000000000, -24.99999999999999645 ) ) ;
#9707 = CARTESIAN_POINT ( 'NONE',  ( -67.56971494453328830, 50.00000002031717372, -0.0004507456344833478141 ) ) ;
#9708 = ORIENTED_EDGE ( 'NONE', *, *, #8792, .F. ) ;
#9709 = CARTESIAN_POINT ( 'NONE',  ( -2.500000000000000000, 3.061616997868383141E-16, -0.3755037691048591086 ) ) ;
#9710 = ORIENTED_EDGE ( 'NONE', *, *, #3131, .F. ) ;
#9711 = ADVANCED_FACE ( 'NONE', ( #1237 ), #515, .T. ) ;
#9712 = CARTESIAN_POINT ( 'NONE',  ( -66.11067862173452170, 48.15427919969674520, 1.842099731909419225 ) ) ;
#9713 = DIRECTION ( 'NONE',  ( 0.8191520442889974607, 1.003171929053531649E-16, -0.5735764363510379438 ) ) ;
#9714 = AXIS2_PLACEMENT_3D ( 'NONE', #8331, #3065, #9409 ) ;
#9715 = CARTESIAN_POINT ( 'NONE',  ( 20.82503005121913731, 76.25610946991470485, 5.714993128054450366 ) ) ;
#9716 = CARTESIAN_POINT ( 'NONE',  ( -73.25000000204838102, 80.81189881250000440, -10.69163855873948954 ) ) ;
#9717 = EDGE_LOOP ( 'NONE', ( #8501, #5457, #5082, #2938 ) ) ;
#9718 = CARTESIAN_POINT ( 'NONE',  ( -77.00000000204838102, 44.30836144126053000, 25.81189881250000795 ) ) ;
#9719 = DIRECTION ( 'NONE',  ( -0.000000000000000000, -0.000000000000000000, -1.000000000000000000 ) ) ;
#9720 = CARTESIAN_POINT ( 'NONE',  ( -78.00000000000002842, 54.99999999999998579, 8.485284746156354529 ) ) ;
#9721 = CARTESIAN_POINT ( 'NONE',  ( -6.090330045190794905, 54.99253937026119843, 0.007033857285447905894 ) ) ;
#9722 = FILL_AREA_STYLE ('',( #1520 ) ) ;
#9723 = DIRECTION ( 'NONE',  ( -0.000000000000000000, -1.000000000000000000, -0.000000000000000000 ) ) ;
#9724 = ORIENTED_EDGE ( 'NONE', *, *, #1765, .T. ) ;
#9725 = DIRECTION ( 'NONE',  ( -1.000000000000000000, -0.000000000000000000, -0.000000000000000000 ) ) ;
#9726 = CARTESIAN_POINT ( 'NONE',  ( -54.00383531698385298, 74.42670172875287449, 8.047314657126378279 ) ) ;
#9727 = EDGE_LOOP ( 'NONE', ( #4939, #5263, #434 ) ) ;
#9728 = CARTESIAN_POINT ( 'NONE',  ( -45.72515810441178274, 68.38234357726757651, -16.29445369018955247 ) ) ;
#9729 = CARTESIAN_POINT ( 'NONE',  ( 1.369680300758778113, 42.32355992005446410, -5.995427644676592394 ) ) ;
#9730 = CARTESIAN_POINT ( 'NONE',  ( -79.43750000204838102, 65.69163855873948421, -25.81189881250000440 ) ) ;
#9731 = VECTOR ( 'NONE', #581, 1000.000000000000000 ) ;
#9732 = AXIS2_PLACEMENT_3D ( 'NONE', #2738, #805, #1818 ) ;
#9733 = EDGE_LOOP ( 'NONE', ( #4736, #6684 ) ) ;
#9734 = CARTESIAN_POINT ( 'NONE',  ( -72.50000000000000000, 55.00000000000000000, -24.99999999999999645 ) ) ;
#9735 = CARTESIAN_POINT ( 'NONE',  ( 7.506399388638331338, 34.30832474160909129, 4.109400874309620200 ) ) ;
#9736 = EDGE_CURVE ( 'NONE', #1195, #4551, #11408, .T. ) ;
#9737 = FACE_OUTER_BOUND ( 'NONE', #5430, .T. ) ;
#9738 = PRESENTATION_LAYER_ASSIGNMENT (  '', '', ( #8140 ) ) ;
#9739 = CARTESIAN_POINT ( 'NONE',  ( 20.70698219299188381, 58.30206649714182277, 3.768798166023678231 ) ) ;
#9740 = CARTESIAN_POINT ( 'NONE',  ( -56.41713135980065630, 60.41248846187414756, 4.441724532788772883 ) ) ;
#9741 = CONICAL_SURFACE ( 'NONE', #4395, 2.999999999999995559, 0.7853981633974420618 ) ;
#9742 = VERTEX_POINT ( 'NONE', #3942 ) ;
#9743 = CARTESIAN_POINT ( 'NONE',  ( 5.969356325850132983, 34.00743083263078859, 1.031241799122481595 ) ) ;
#9744 = CARTESIAN_POINT ( 'NONE',  ( -15.00000000000000355, 0.000000000000000000, -29.99999999999999289 ) ) ;
#9745 = FACE_OUTER_BOUND ( 'NONE', #7300, .T. ) ;
#9746 = EDGE_CURVE ( 'NONE', #11526, #19, #1088, .T. ) ;
#9747 = CYLINDRICAL_SURFACE ( 'NONE', #1130, 24.99999999999999645 ) ;
#9748 = CARTESIAN_POINT ( 'NONE',  ( -73.81250000204839523, 29.18810118750000981, 10.69163855873950020 ) ) ;
#9749 = ORIENTED_EDGE ( 'NONE', *, *, #3285, .T. ) ;
#9750 = CARTESIAN_POINT ( 'NONE',  ( -71.18750000409677625, 72.67766952966368876, -17.67766952966368876 ) ) ;
#9751 = CARTESIAN_POINT ( 'NONE',  ( -78.00000000000001421, 63.48528137423857487, -8.485278002320759683 ) ) ;
#9752 = CARTESIAN_POINT ( 'NONE',  ( -78.00000000000002842, 54.99999999999998579, 6.985284746156355418 ) ) ;
#9753 = AXIS2_PLACEMENT_3D ( 'NONE', #9826, #2527, #1615 ) ;
#9754 = CARTESIAN_POINT ( 'NONE',  ( 2.826857198123298165, 37.44742646213195769, -11.71858918393001225 ) ) ;
#9755 = VERTEX_POINT ( 'NONE', #9685 ) ;
#9756 = CARTESIAN_POINT ( 'NONE',  ( -77.56250000204838102, 80.81189881250000440, 10.69163855873948243 ) ) ;
#9757 = CARTESIAN_POINT ( 'NONE',  ( -15.00000000000000000, -24.99999999999999645, 10.00000000000000000 ) ) ;
#9758 = CARTESIAN_POINT ( 'NONE',  ( 0.000000000000000000, 0.000000000000000000, -0.02539999999999996774 ) ) ;
#9759 = AXIS2_PLACEMENT_3D ( 'NONE', #10045, #9158, #8384 ) ;
#9760 = CARTESIAN_POINT ( 'NONE',  ( -24.47759590008010377, 52.25445690686086664, 21.01882782503509262 ) ) ;
#9761 = CYLINDRICAL_SURFACE ( 'NONE', #10922, 24.99999999999999645 ) ;
#9762 = CARTESIAN_POINT ( 'NONE',  ( -78.78125000204838102, 55.00000000000000000, 25.81189881249999729 ) ) ;
#9763 = CARTESIAN_POINT ( 'NONE',  ( 4.999999999999998224, -2.886751345948137981, -0.4465819873852071575 ) ) ;
#9764 = EDGE_LOOP ( 'NONE', ( #11322, #9533, #1303, #3713 ) ) ;
#9765 = CARTESIAN_POINT ( 'NONE',  ( 53.00000000000000000, 51.46446609406726935, 3.535533905932731091 ) ) ;
#9766 = AXIS2_PLACEMENT_3D ( 'NONE', #1021, #6617, #10961 ) ;
#9767 = VERTEX_POINT ( 'NONE', #10402 ) ;
#9768 = ADVANCED_FACE ( 'NONE', ( #11234, #7777 ), #5869, .T. ) ;
#9769 = CARTESIAN_POINT ( 'NONE',  ( -60.08385138347627219, 52.96922280571201469, 6.695818664272940701 ) ) ;
#9770 = AXIS2_PLACEMENT_3D ( 'NONE', #3049, #2932, #6600 ) ;
#9771 = CARTESIAN_POINT ( 'NONE',  ( 9.999999999999994671, 0.000000000000000000, 10.00000000000000000 ) ) ;
#9772 = CARTESIAN_POINT ( 'NONE',  ( -14.70500487297517189, 60.00000000000030553, -0.3308759158401262668 ) ) ;
#9773 = DIRECTION ( 'NONE',  ( 0.000000000000000000, 0.000000000000000000, 1.000000000000000000 ) ) ;
#9774 = CARTESIAN_POINT ( 'NONE',  ( 21.36699128324961805, 76.70829236948175378, 3.640766976057809856 ) ) ;
#9775 = CONICAL_SURFACE ( 'NONE', #9199, 3.000000000000000000, 0.9599310885968912466 ) ;
#9776 = AXIS2_PLACEMENT_3D ( 'NONE', #8763, #5171, #11439 ) ;
#9777 = CARTESIAN_POINT ( 'NONE',  ( 4.999999999999999112, 0.4881033300985028744, -6.099999999999999645 ) ) ;
#9778 = ORIENTED_EDGE ( 'NONE', *, *, #1054, .F. ) ;
#9779 = CARTESIAN_POINT ( 'NONE',  ( -75.59375000204839523, 55.00000000000000000, 25.81189881249999729 ) ) ;
#9780 = DIRECTION ( 'NONE',  ( 0.000000000000000000, 1.000000000000000000, 0.000000000000000000 ) ) ;
#9781 = CARTESIAN_POINT ( 'NONE',  ( 4.997868933204849817, 55.00264723353835450, 0.001346135474403307910 ) ) ;
#9782 = AXIS2_PLACEMENT_3D ( 'NONE', #9213, #3527, #5334 ) ;
#9783 = SURFACE_STYLE_USAGE ( .BOTH. , #11572 ) ;
#9784 = CIRCLE ( 'NONE', #3292, 20.00000000000000355 ) ;
#9785 = CARTESIAN_POINT ( 'NONE',  ( -75.00000000000001421, 31.01194267615668920, 8.057582179793557842 ) ) ;
#9786 = EDGE_CURVE ( 'NONE', #9107, #8222, #2048, .T. ) ;
#9787 = VERTEX_POINT ( 'NONE', #4178 ) ;
#9788 = CARTESIAN_POINT ( 'NONE',  ( -78.00000000000001421, 50.75735931288069480, -4.242637315201482906 ) ) ;
#9789 = CARTESIAN_POINT ( 'NONE',  ( -59.27472368810988002, 61.13901599248961105, 20.20251803659174783 ) ) ;
#9790 = EDGE_LOOP ( 'NONE', ( #484, #8362, #6245, #5137 ) ) ;
#9791 = CARTESIAN_POINT ( 'NONE',  ( -32.32947787139347895, 33.97704578748628990, 0.0005171865318368603498 ) ) ;
#9792 = CARTESIAN_POINT ( 'NONE',  ( -20.21146696499166140, 63.35170862394775071, 11.26075774480146485 ) ) ;
#9793 = CARTESIAN_POINT ( 'NONE',  ( -79.06250000204839523, 80.81189881250001861, 10.69163855873948599 ) ) ;
#9794 = ORIENTED_EDGE ( 'NONE', *, *, #10688, .F. ) ;
#9795 = CARTESIAN_POINT ( 'NONE',  ( -73.53125000000000000, 80.00000000000001421, 10.35533905932737397 ) ) ;
#9796 = CARTESIAN_POINT ( 'NONE',  ( 8.058385817489730485, 34.79396711235183659, 6.140502173211014103 ) ) ;
#9797 = EDGE_CURVE ( 'NONE', #8631, #11604, #8179, .T. ) ;
#9798 = CYLINDRICAL_SURFACE ( 'NONE', #7453, 25.00000000000000355 ) ;
#9799 = CARTESIAN_POINT ( 'NONE',  ( 23.03641490397931335, 59.49166983161503452, 2.221310855399595496 ) ) ;
#9800 = CARTESIAN_POINT ( 'NONE',  ( -65.75072559461156629, 50.54239926659131044, 5.429416014682115765 ) ) ;
#9801 = ORIENTED_EDGE ( 'NONE', *, *, #8196, .T. ) ;
#9802 = CARTESIAN_POINT ( 'NONE',  ( 5.662790106042886684, 33.97208755798592961, -0.0004309138471297446066 ) ) ;
#9803 = DIRECTION ( 'NONE',  ( 0.000000000000000000, 1.000000000000000000, 0.000000000000000000 ) ) ;
#9804 = DIRECTION ( 'NONE',  ( -1.000000000000000000, -0.000000000000000000, -0.000000000000000000 ) ) ;
#9805 = FACE_OUTER_BOUND ( 'NONE', #7852, .T. ) ;
#9806 = CARTESIAN_POINT ( 'NONE',  ( -71.34302368722833876, 77.35376350879521112, 12.90594348738575903 ) ) ;
#9807 = ORIENTED_EDGE ( 'NONE', *, *, #11024, .T. ) ;
#9808 = FACE_OUTER_BOUND ( 'NONE', #1651, .T. ) ;
#9809 = DIRECTION ( 'NONE',  ( 1.000000000000000000, 0.000000000000000000, 0.000000000000000000 ) ) ;
#9810 = PRODUCT_DEFINITION ( 'UNKNOWN', '', #11379, #4266 ) ;
#9811 = FACE_BOUND ( 'NONE', #7629, .T. ) ;
#9812 = EDGE_CURVE ( 'NONE', #4918, #4978, #5086, .T. ) ;
#9813 = EDGE_CURVE ( 'NONE', #1264, #8509, #11603, .T. ) ;
#9814 = CARTESIAN_POINT ( 'NONE',  ( -52.59603425219209782, 73.55155261293346314, 9.913157997185967574 ) ) ;
#9815 = EDGE_CURVE ( 'NONE', #10744, #8509, #6887, .T. ) ;
#9816 = ORIENTED_EDGE ( 'NONE', *, *, #9081, .T. ) ;
#9817 = DIRECTION ( 'NONE',  ( 1.000000000000000000, 0.000000000000000000, 0.000000000000000000 ) ) ;
#9818 = FACE_BOUND ( 'NONE', #6411, .T. ) ;
#9819 = CYLINDRICAL_SURFACE ( 'NONE', #2649, 1.500000000000000000 ) ;
#9820 = AXIS2_PLACEMENT_3D ( 'NONE', #7546, #10283, #11167 ) ;
#9821 = EDGE_CURVE ( 'NONE', #7952, #5798, #4968, .T. ) ;
#9822 = EDGE_CURVE ( 'NONE', #4492, #8007, #3586, .T. ) ;
#9823 = CARTESIAN_POINT ( 'NONE',  ( 19.51996453321225644, 59.49466458524579338, 2.214906497190253010 ) ) ;
#9824 = CARTESIAN_POINT ( 'NONE',  ( -80.00000000000000000, 55.00000000000000000, -24.99999999999999645 ) ) ;
#9825 = CARTESIAN_POINT ( 'NONE',  ( -75.50000000204840944, 29.18810118750000981, 10.69163855873950020 ) ) ;
#9826 = CARTESIAN_POINT ( 'NONE',  ( -78.00000000000001421, 46.51471862576140381, -8.485278002320759683 ) ) ;
#9827 = ORIENTED_EDGE ( 'NONE', *, *, #7718, .T. ) ;
#9828 = EDGE_CURVE ( 'NONE', #1911, #3047, #3277, .T. ) ;
#9829 = DIRECTION ( 'NONE',  ( 0.000000000000000000, 1.000000000000000000, 0.000000000000000000 ) ) ;
#9830 = VERTEX_POINT ( 'NONE', #6715 ) ;
#9831 = CARTESIAN_POINT ( 'NONE',  ( -45.10988329347496517, 60.61560339207529324, -4.319777640813139641 ) ) ;
#9832 = VECTOR ( 'NONE', #3114, 1000.000000000000000 ) ;
#9833 = CARTESIAN_POINT ( 'NONE',  ( -70.87427368927673399, 76.65063840437989029, 12.49999426731031704 ) ) ;
#9834 = CARTESIAN_POINT ( 'NONE',  ( -76.62500000409677625, 55.00000000000000000, 24.99999999999999645 ) ) ;
#9835 = FACE_OUTER_BOUND ( 'NONE', #7019, .T. ) ;
#9836 = CARTESIAN_POINT ( 'NONE',  ( -73.43750000204839523, 65.69163855873948421, -25.81189881250000084 ) ) ;
#9837 = ORIENTED_EDGE ( 'NONE', *, *, #10967, .F. ) ;
#9838 = CARTESIAN_POINT ( 'NONE',  ( -77.09375000204839523, 55.00000000000000000, 25.81189881249999729 ) ) ;
#9839 = CARTESIAN_POINT ( 'NONE',  ( -5.000000000000000888, 0.000000000000000000, 0.000000000000000000 ) ) ;
#9840 = CARTESIAN_POINT ( 'NONE',  ( -77.37500000409677625, 55.00000000000000000, -24.99999999999999645 ) ) ;
#9841 = CARTESIAN_POINT ( 'NONE',  ( -6.668797733382348270, 54.99774328067935159, 0.001930581088264634107 ) ) ;
#9842 = CARTESIAN_POINT ( 'NONE',  ( -78.00000000000002842, 59.24264068711927678, 12.72792543327563131 ) ) ;
#9843 = VERTEX_POINT ( 'NONE', #279 ) ;
#9844 = DIRECTION ( 'NONE',  ( 1.000000000000000000, 0.000000000000000000, 0.000000000000000000 ) ) ;
#9845 = DIRECTION ( 'NONE',  ( 0.000000000000000000, 0.000000000000000000, 1.000000000000000000 ) ) ;
#9846 = ORIENTED_EDGE ( 'NONE', *, *, #3169, .F. ) ;
#9847 = CARTESIAN_POINT ( 'NONE',  ( -44.30269363598408461, 63.99200565043310007, -19.01284557474750514 ) ) ;
#9848 = CARTESIAN_POINT ( 'NONE',  ( -75.87500000204839523, 65.69163855873949842, 25.81189881250000440 ) ) ;
#9849 = MECHANICAL_DESIGN_GEOMETRIC_PRESENTATION_REPRESENTATION (  '', ( #477 ), #1235 ) ;
#9850 = AXIS2_PLACEMENT_3D ( 'NONE', #5806, #452, #8492 ) ;
#9851 = ORIENTED_EDGE ( 'NONE', *, *, #3740, .F. ) ;
#9852 = CARTESIAN_POINT ( 'NONE',  ( -73.62500000204839523, 44.30836144126050158, -25.81189881249999374 ) ) ;
#9853 = DIRECTION ( 'NONE',  ( 0.000000000000000000, 1.000000000000000000, 0.000000000000000000 ) ) ;
#9854 = EDGE_LOOP ( 'NONE', ( #4126, #8181, #9324, #74 ) ) ;
#9855 = CARTESIAN_POINT ( 'NONE',  ( 0.000000000000000000, 5.773502691896260863, -5.653418012614792154 ) ) ;
#9856 = CARTESIAN_POINT ( 'NONE',  ( 14.87104979758787771, 53.70723891340239220, 4.840877117755912451 ) ) ;
#9857 = CARTESIAN_POINT ( 'NONE',  ( -8.047727199116865293, 54.99755268931162533, 0.004974585571924257203 ) ) ;
#9858 = VERTEX_POINT ( 'NONE', #8620 ) ;
#9859 = CARTESIAN_POINT ( 'NONE',  ( -12.18906244258289995, 75.97791289299129858, -2.745668048143513396 ) ) ;
#9860 = CARTESIAN_POINT ( 'NONE',  ( -30.36397657560652874, 35.99904827701746513, 8.986701095552454888 ) ) ;
#9861 = CARTESIAN_POINT ( 'NONE',  ( 6.123233995736766282E-16, -24.99999999999999645, 5.000000000000000000 ) ) ;
#9862 = LINE ( 'NONE', #10755, #6120 ) ;
#9863 = DIRECTION ( 'NONE',  ( -1.000000000000000000, 0.000000000000000000, 0.000000000000000000 ) ) ;
#9864 = VERTEX_POINT ( 'NONE', #402 ) ;
#9865 = CARTESIAN_POINT ( 'NONE',  ( -71.28125000409677625, 65.35533905932737753, -24.99999999999999645 ) ) ;
#9866 = DIRECTION ( 'NONE',  ( -1.000000000000000000, -0.000000000000000000, -0.000000000000000000 ) ) ;
#9867 = CARTESIAN_POINT ( 'NONE',  ( -71.75000000409677625, 30.00000000000000355, 4.592425496802573578E-15 ) ) ;
#9868 = VECTOR ( 'NONE', #6836, 1000.000000000000000 ) ;
#9869 = CARTESIAN_POINT ( 'NONE',  ( -61.32723930490969622, 46.95308112547827051, 19.41976192622660946 ) ) ;
#9870 = VERTEX_POINT ( 'NONE', #8499 ) ;
#9871 = FACE_OUTER_BOUND ( 'NONE', #3080, .T. ) ;
#9872 = CARTESIAN_POINT ( 'NONE',  ( -78.87500000409677625, 55.00000000000000000, -24.99999999999999645 ) ) ;
#9873 = VERTEX_POINT ( 'NONE', #11354 ) ;
#9874 = CARTESIAN_POINT ( 'NONE',  ( -78.00000000000001421, 59.24264068711927678, -4.242637315201482906 ) ) ;
#9875 = CARTESIAN_POINT ( 'NONE',  ( 7.851389403161795677, 51.23265128290481840, 3.303652424085503636 ) ) ;
#9876 = CARTESIAN_POINT ( 'NONE',  ( -71.91717626682689968, 72.42551787026226862, 19.81812247078860523 ) ) ;
#9877 = LINE ( 'NONE', #1673, #2679 ) ;
#9878 = EDGE_LOOP ( 'NONE', ( #11543, #11453, #6958 ) ) ;
#9879 = CIRCLE ( 'NONE', #5884, 1.500000000000001332 ) ;
#9880 = FACE_OUTER_BOUND ( 'NONE', #7987, .T. ) ;
#9881 = VERTEX_POINT ( 'NONE', #10347 ) ;
#9882 = CARTESIAN_POINT ( 'NONE',  ( 7.095683716263478047, 50.00000000000005684, 2.757939276259992832E-15 ) ) ;
#9883 = AXIS2_PLACEMENT_3D ( 'NONE', #4731, #9458, #3768 ) ;
#9884 = CARTESIAN_POINT ( 'NONE',  ( -5.001868413209209940, 60.36545409722314304, -12.95245650687548356 ) ) ;
#9885 = ADVANCED_FACE ( 'NONE', ( #5031 ), #3162, .F. ) ;
#9886 = CARTESIAN_POINT ( 'NONE',  ( -76.34375000204839523, 55.00000000000000000, -25.81189881249999729 ) ) ;
#9887 = LINE ( 'NONE', #9112, #7031 ) ;
#9888 = DIRECTION ( 'NONE',  ( 0.000000000000000000, 1.000000000000000000, 0.000000000000000000 ) ) ;
#9889 = CIRCLE ( 'NONE', #7616, 5.249999999999998224 ) ;
#9890 = CARTESIAN_POINT ( 'NONE',  ( -78.00000000000002842, 42.27207793864211283, 4.242644059037075976 ) ) ;
#9891 = VECTOR ( 'NONE', #5017, 1000.000000000000000 ) ;
#9892 = EDGE_LOOP ( 'NONE', ( #10751, #1638, #396, #11553 ) ) ;
#9893 = CARTESIAN_POINT ( 'NONE',  ( 0.8179331680532999638, 5.301268757141563093, -0.1739375980333749683 ) ) ;
#9894 = ADVANCED_FACE ( 'NONE', ( #8677 ), #9451, .F. ) ;
#9895 = CARTESIAN_POINT ( 'NONE',  ( -73.90625000204839523, 36.74823131438026280, 18.25176868561974786 ) ) ;
#9896 = EDGE_CURVE ( 'NONE', #3359, #8432, #4157, .T. ) ;
#9897 = LINE ( 'NONE', #6205, #2112 ) ;
#9898 = CARTESIAN_POINT ( 'NONE',  ( 3.000000000000000000, 3.673940397442059868E-16, -0.02539999999999996774 ) ) ;
#9899 = CARTESIAN_POINT ( 'NONE',  ( -29.42366337843931490, 55.01024914994471260, 0.0003017736481339514825 ) ) ;
#9900 = CARTESIAN_POINT ( 'NONE',  ( 0.000000000000000000, 0.000000000000000000, 0.000000000000000000 ) ) ;
#9901 = AXIS2_PLACEMENT_3D ( 'NONE', #1202, #10118, #9230 ) ;
#9902 = CARTESIAN_POINT ( 'NONE',  ( -75.00000000000001421, 29.78398716281686021, 3.536572121053506823 ) ) ;
#9903 = ORIENTED_EDGE ( 'NONE', *, *, #6156, .F. ) ;
#9904 = CARTESIAN_POINT ( 'NONE',  ( -15.46272266344517909, 58.97603181275015771, 3.049243307324925656 ) ) ;
#9905 = FACE_OUTER_BOUND ( 'NONE', #9559, .T. ) ;
#9906 = VERTEX_POINT ( 'NONE', #11528 ) ;
#9907 = CARTESIAN_POINT ( 'NONE',  ( -53.92936707256667717, 73.55041509984243930, 9.912644826577484025 ) ) ;
#9908 = CARTESIAN_POINT ( 'NONE',  ( -76.25000000204838102, 80.81189881250001861, -10.69163855873949132 ) ) ;
#9909 = AXIS2_PLACEMENT_3D ( 'NONE', #10647, #4987, #1500 ) ;
#9910 = ORIENTED_EDGE ( 'NONE', *, *, #3072, .F. ) ;
#9911 = CARTESIAN_POINT ( 'NONE',  ( -76.15625000204838102, 80.81189881250000440, -1.580522963032174394E-15 ) ) ;
#9912 = CARTESIAN_POINT ( 'NONE',  ( 25.76190476190475565, 59.99999999999995026, 0.000000000000000000 ) ) ;
#9913 = ADVANCED_FACE ( 'NONE', ( #8854 ), #5890, .F. ) ;
#9914 = CARTESIAN_POINT ( 'NONE',  ( -80.00000000000001421, 67.72792206135787296, -14.22791868944004356 ) ) ;
#9915 = DIRECTION ( 'NONE',  ( 0.000000000000000000, 0.000000000000000000, 1.000000000000000000 ) ) ;
#9916 = CARTESIAN_POINT ( 'NONE',  ( -0.1631717787953173293, 54.99775794017483577, -0.001150061841714329494 ) ) ;
#9917 = VERTEX_POINT ( 'NONE', #8971 ) ;
#9918 = CARTESIAN_POINT ( 'NONE',  ( -58.69833756168564065, 56.03204939003842355, 20.99267139547387373 ) ) ;
#9919 = CARTESIAN_POINT ( 'NONE',  ( -30.67054324275970600, 35.57292846186890500, 8.046485333435041909 ) ) ;
#9920 = SURFACE_STYLE_USAGE ( .BOTH. , #8193 ) ;
#9921 = VECTOR ( 'NONE', #3885, 1000.000000000000000 ) ;
#9922 = DIRECTION ( 'NONE',  ( -1.000000000000000000, 0.000000000000000000, 0.000000000000000000 ) ) ;
#9923 = DIRECTION ( 'NONE',  ( -1.000000000000000000, -0.000000000000000000, -0.000000000000000000 ) ) ;
#9924 = ORIENTED_EDGE ( 'NONE', *, *, #522, .F. ) ;
#9925 = LINE ( 'NONE', #9091, #6532 ) ;
#9926 = CARTESIAN_POINT ( 'NONE',  ( 39.99999999999999289, 55.00000000000000000, -24.99999999999999645 ) ) ;
#9927 = CARTESIAN_POINT ( 'NONE',  ( 19.99999999999996803, -63.00000000000000000, 5.000000000000000000 ) ) ;
#9928 = VECTOR ( 'NONE', #409, 1000.000000000000000 ) ;
#9929 = VERTEX_POINT ( 'NONE', #4295 ) ;
#9930 = DIRECTION ( 'NONE',  ( 1.000000000000000000, 6.033820786006286457E-17, -0.000000000000000000 ) ) ;
#9931 = VECTOR ( 'NONE', #1285, 1000.000000000000000 ) ;
#9932 = EDGE_CURVE ( 'NONE', #10233, #2213, #4548, .T. ) ;
#9933 = CARTESIAN_POINT ( 'NONE',  ( -53.21169738097692203, 59.96713617643348471, 0.6587253374105324077 ) ) ;
#9934 = ORIENTED_EDGE ( 'NONE', *, *, #3572, .T. ) ;
#9935 = CARTESIAN_POINT ( 'NONE',  ( 36.99999999999999289, 45.00000000000001421, 1.224646799147351679E-15 ) ) ;
#9936 = CYLINDRICAL_SURFACE ( 'NONE', #8356, 2.500000000000000000 ) ;
#9937 = EDGE_CURVE ( 'NONE', #11519, #8176, #2440, .T. ) ;
#9938 = CARTESIAN_POINT ( 'NONE',  ( -79.06250000204839523, 80.81189881250001861, 10.69163855873948599 ) ) ;
#9939 = FACE_OUTER_BOUND ( 'NONE', #3487, .T. ) ;
#9940 = AXIS2_PLACEMENT_3D ( 'NONE', #6739, #5715, #4991 ) ;
#9941 = ORIENTED_EDGE ( 'NONE', *, *, #8792, .T. ) ;
#9942 = CARTESIAN_POINT ( 'NONE',  ( -76.15625000204839523, 73.25176868561975141, -18.25176868561974430 ) ) ;
#9943 = EDGE_LOOP ( 'NONE', ( #9851, #8760, #2792, #5049 ) ) ;
#9944 = CARTESIAN_POINT ( 'NONE',  ( 0.8592290948358244362, 65.44860072268932072, 22.71185887947197557 ) ) ;
#9945 = CARTESIAN_POINT ( 'NONE',  ( -1.127104549820378221, 51.32464662373498498, -13.65769093838479442 ) ) ;
#9946 = EDGE_CURVE ( 'NONE', #10425, #3280, #4239, .T. ) ;
#9947 = CARTESIAN_POINT ( 'NONE',  ( -78.50000000204842365, 44.30836144126052289, 25.81189881250000795 ) ) ;
#9948 = CARTESIAN_POINT ( 'NONE',  ( 0.3675172377051636463, 64.99605696851787684, -19.59792961213366169 ) ) ;
#9949 = CARTESIAN_POINT ( 'NONE',  ( -73.15625000204838102, 80.81189881250000440, -1.580522963032174394E-15 ) ) ;
#9950 = ORIENTED_EDGE ( 'NONE', *, *, #2693, .F. ) ;
#9951 =( LENGTH_UNIT ( ) NAMED_UNIT ( * ) SI_UNIT ( .MILLI., .METRE. ) );
#9952 = CARTESIAN_POINT ( 'NONE',  ( -78.78125000409679046, 65.35533905932737753, -24.99999999999999645 ) ) ;
#9953 = EDGE_CURVE ( 'NONE', #4670, #3266, #6662, .T. ) ;
#9954 = CARTESIAN_POINT ( 'NONE',  ( -4.999999999999999112, 0.4881033300985023748, 4.497744949920333814E-16 ) ) ;
#9955 = CARTESIAN_POINT ( 'NONE',  ( -77.28125000409677625, 65.35533905932743437, -24.99999999999994671 ) ) ;
#9956 = CARTESIAN_POINT ( 'NONE',  ( -49.23625742515549319, 55.01965444600840272, 0.001248010823296030226 ) ) ;
#9957 = DIRECTION ( 'NONE',  ( 1.000000000000000000, 6.033820786006286457E-17, -0.000000000000000000 ) ) ;
#9958 = VECTOR ( 'NONE', #6179, 1000.000000000000000 ) ;
#9959 = AXIS2_PLACEMENT_3D ( 'NONE', #3311, #6079, #5287 ) ;
#9960 = CARTESIAN_POINT ( 'NONE',  ( -9.624147497243844995, 59.74499220970398028, -1.610198918108491029 ) ) ;
#9961 = CARTESIAN_POINT ( 'NONE',  ( -62.45014759628331547, 49.89181376149021219, 20.39015500988638507 ) ) ;
#9962 = VERTEX_POINT ( 'NONE', #5318 ) ;
#9963 = CARTESIAN_POINT ( 'NONE',  ( -31.73741350946478335, 34.08379956678489009, 2.058435976334235473 ) ) ;
#9964 = CARTESIAN_POINT ( 'NONE',  ( -75.40625000204838102, 29.18810118750000271, 4.741568889096522788E-15 ) ) ;
#9965 = VECTOR ( 'NONE', #2984, 1000.000000000000000 ) ;
#9966 = CIRCLE ( 'NONE', #6557, 4.999999999999997335 ) ;
#9967 = VERTEX_POINT ( 'NONE', #8908 ) ;
#9968 = EDGE_CURVE ( 'NONE', #10943, #8444, #7394, .T. ) ;
#9969 = CARTESIAN_POINT ( 'NONE',  ( -73.71875000204839523, 36.74823131438024859, -18.25176868561973720 ) ) ;
#9970 = CARTESIAN_POINT ( 'NONE',  ( -28.36397722366938012, 36.00052710555507218, 8.986026874162561739 ) ) ;
#9971 =( BOUNDED_CURVE ( )  B_SPLINE_CURVE ( 2, ( #1134, #2096, #417, #4079, #4802, #8460, #10182, #238, #5829, #5769, #7679, #11315, #3123, #6788, #2218, #7738, #6184, #10589, #532, #7915, #2390, #9756, #4377, #11544, #2456, #7795, #4256, #6122, #3348, #6964, #7020, #4311, #1498, #3410, #11485, #10643, #6066, #6904, #8029, #649, #8869, #5221, #7969, #4195, #5157, #1555, #3295, #11605, #705, #7083, #3178 ),
 .UNSPECIFIED., .F., .T. ) 
 B_SPLINE_CURVE_WITH_KNOTS ( ( 3, 2, 2, 2, 2, 2, 2, 2, 2, 2, 2, 2, 2, 2, 2, 2, 2, 2, 2, 2, 2, 2, 2, 2, 2, 3 ),
 ( 0.000000000000000000, 0.02083333333333333218, 0.04166666666666666435, 0.06250000000000000000, 0.08333333333333332871, 0.1041666666666666713, 0.1250000000000000000, 0.1458333333333333426, 0.1666666666666666574, 0.1875000000000000000, 0.2083333333333333426, 0.2291666666666666574, 0.2500000000000000000, 0.2708333333333333148, 0.2916666666666666852, 0.3125000000000000000, 0.3333333333333333148, 0.3541666666666666852, 0.3750000000000000000, 0.3958333333333333148, 0.4166666666666666852, 0.4375000000000000000, 0.4583333333333333148, 0.4791666666666666852, 0.5000000000000000000, 0.5036241432350977432 ),
 .UNSPECIFIED. ) 
 CURVE ( )  GEOMETRIC_REPRESENTATION_ITEM ( )  RATIONAL_B_SPLINE_CURVE ( ( 1.000000000000000000, 0.9238795325112867385, 1.000000000000000000, 0.9238795325112867385, 1.000000000000000000, 0.9238795325112867385, 1.000000000000000000, 0.9238795325112867385, 1.000000000000000000, 0.9238795325112867385, 1.000000000000000000, 0.9238795325112867385, 1.000000000000000000, 0.9238795325112867385, 1.000000000000000000, 0.9238795325112867385, 1.000000000000000000, 0.9238795325112867385, 1.000000000000000000, 0.9238795325112867385, 1.000000000000000000, 0.9238795325112867385, 1.000000000000000000, 0.9238795325112867385, 1.000000000000000000, 0.9238795325112867385, 1.000000000000000000, 0.9238795325112867385, 1.000000000000000000, 0.9238795325112867385, 1.000000000000000000, 0.9238795325112867385, 1.000000000000000000, 0.9238795325112867385, 1.000000000000000000, 0.9238795325112867385, 1.000000000000000000, 0.9238795325112867385, 1.000000000000000000, 0.9238795325112867385, 1.000000000000000000, 0.9238795325112867385, 1.000000000000000000, 0.9238795325112867385, 1.000000000000000000, 0.9238795325112867385, 1.000000000000000000, 0.9238795325112867385, 1.000000000000000000, 0.9867581690895185220, 0.9781234062028318910 ) ) 
 REPRESENTATION_ITEM ( '' )  );
#9972 = EDGE_LOOP ( 'NONE', ( #11731, #6950, #1699, #4082 ) ) ;
#9973 = FACE_OUTER_BOUND ( 'NONE', #9733, .T. ) ;
#9974 = CARTESIAN_POINT ( 'NONE',  ( -8.331185513520907193, 55.00093008094477653, -0.001764911158480240083 ) ) ;
#9975 = ORIENTED_EDGE ( 'NONE', *, *, #8008, .F. ) ;
#9976 = CARTESIAN_POINT ( 'NONE',  ( 0.1890707644848960145, 42.07652144655710913, -16.80626323592864324 ) ) ;
#9977 = CARTESIAN_POINT ( 'NONE',  ( -29.49360042904642043, 37.45509264529403737, 11.71531283165970727 ) ) ;
#9978 = CARTESIAN_POINT ( 'NONE',  ( 39.99999999999999289, 55.00000000000000000, 0.000000000000000000 ) ) ;
#9979 = LINE ( 'NONE', #10986, #11664 ) ;
#9980 = ADVANCED_BREP_SHAPE_REPRESENTATION ( '', ( #8858, #4738 ), #3015 ) ;
#9981 = ORIENTED_EDGE ( 'NONE', *, *, #5718, .F. ) ;
#9982 = DIRECTION ( 'NONE',  ( 1.000000000000000000, 6.033820786006286457E-17, -0.000000000000000000 ) ) ;
#9983 = CARTESIAN_POINT ( 'NONE',  ( -45.09032857029786356, 54.99712218131477925, 0.005861851983533778246 ) ) ;
#9984 = CARTESIAN_POINT ( 'NONE',  ( -31.79252387391919754, 50.12764572993967249, -1.301498629944670249 ) ) ;
#9985 = ORIENTED_EDGE ( 'NONE', *, *, #9673, .T. ) ;
#9986 = B_SPLINE_CURVE_WITH_KNOTS ( 'NONE', 3,
 ( #11213, #1217, #1157, #4884, #8351, #8479 ),
 .UNSPECIFIED., .F., .F.,
 ( 4, 2, 4 ),
 ( 0.008070708573309217163, 0.009531758523483289253, 0.01099280847365736134 ),
 .UNSPECIFIED. ) ;
#9987 = CARTESIAN_POINT ( 'NONE',  ( 36.99999999999999289, 55.00000000000000000, 0.000000000000000000 ) ) ;
#9988 = CARTESIAN_POINT ( 'NONE',  ( -63.70414766735607515, 53.39330387528737987, 4.746099453471545715 ) ) ;
#9989 = VERTEX_POINT ( 'NONE', #11328 ) ;
#9990 = CARTESIAN_POINT ( 'NONE',  ( -72.50000000000000000, 55.00000000000000000, -24.99999999999999645 ) ) ;
#9991 = CARTESIAN_POINT ( 'NONE',  ( -31.04449509981424526, 50.50450958133799872, 2.213278473101321087 ) ) ;
#9992 = CARTESIAN_POINT ( 'NONE',  ( -68.81799204399976588, 34.52608862562686909, 5.501299279293338174 ) ) ;
#9993 = CARTESIAN_POINT ( 'NONE',  ( -72.12500000204839523, 44.30836144126050158, -25.81189881249999374 ) ) ;
#9994 = CARTESIAN_POINT ( 'NONE',  ( -78.12500000204838102, 44.30836144126050158, -25.81189881249999374 ) ) ;
#9995 = ORIENTED_EDGE ( 'NONE', *, *, #7486, .F. ) ;
#9996 = CARTESIAN_POINT ( 'NONE',  ( -77.09375000204839523, 55.00000000000000000, 25.81189881249999729 ) ) ;
#9997 = ORIENTED_EDGE ( 'NONE', *, *, #7600, .F. ) ;
#9998 = CARTESIAN_POINT ( 'NONE',  ( -1.262803747101160834, 54.17797665385903372, -4.934652714417677721 ) ) ;
#9999 = CARTESIAN_POINT ( 'NONE',  ( 0.4604261215510325744, 47.96020507958075285, -12.21094979895113219 ) ) ;
#10000 = CARTESIAN_POINT ( 'NONE',  ( -75.01598058408755776, 37.97957837300059225, -19.48311574424008086 ) ) ;
#10001 = EDGE_CURVE ( 'NONE', #10874, #9124, #6855, .T. ) ;
#10002 = EDGE_CURVE ( 'NONE', #1948, #1442, #6685, .T. ) ;
#10003 = CARTESIAN_POINT ( 'NONE',  ( 3.351853367131007122, -3.838309248099025961, -6.099999999999998757 ) ) ;
#10004 = EDGE_LOOP ( 'NONE', ( #5027, #2868, #6336, #7924, #6209 ) ) ;
#10005 =( LENGTH_UNIT ( ) NAMED_UNIT ( * ) SI_UNIT ( .MILLI., .METRE. ) );
#10006 = CARTESIAN_POINT ( 'NONE',  ( -76.81250000409679046, 72.67766952966368876, 17.67766952966368521 ) ) ;
#10007 = EDGE_CURVE ( 'NONE', #3733, #1955, #3205, .T. ) ;
#10008 = CARTESIAN_POINT ( 'NONE',  ( 47.00000000000000000, 51.46446609406726935, 3.535533905932731091 ) ) ;
#10009 = CARTESIAN_POINT ( 'NONE',  ( -41.66879782724831927, 54.99865377049987103, 0.002647339441117046391 ) ) ;
#10010 = CARTESIAN_POINT ( 'NONE',  ( -2.541277572167694121, 65.22933659532863260, -19.47729156647515936 ) ) ;
#10011 = CARTESIAN_POINT ( 'NONE',  ( -11.18084273084829583, 59.99169012976696536, -0.3319299593735249854 ) ) ;
#10012 = ORIENTED_EDGE ( 'NONE', *, *, #3400, .T. ) ;
#10013 = CIRCLE ( 'NONE', #4872, 1.500000000000001332 ) ;
#10014 = CARTESIAN_POINT ( 'NONE',  ( 4.180704885107411783, 3.359771601077107483, -0.1983443223721572113 ) ) ;
#10015 = ORIENTED_EDGE ( 'NONE', *, *, #7600, .T. ) ;
#10016 = CARTESIAN_POINT ( 'NONE',  ( -8.214759031591983174, 65.81066618478850216, -18.03675305545087681 ) ) ;
#10017 = PRODUCT_RELATED_PRODUCT_CATEGORY ( 'part', '', ( #10824 ) ) ;
#10018 = CARTESIAN_POINT ( 'NONE',  ( -72.50000000204839523, 29.18810118750000981, 10.69163855873950020 ) ) ;
#10019 = EDGE_CURVE ( 'NONE', #9403, #7593, #5702, .T. ) ;
#10020 = ORIENTED_EDGE ( 'NONE', *, *, #10909, .T. ) ;
#10021 = CARTESIAN_POINT ( 'NONE',  ( -74.75000000204839523, 80.81189881250001861, -10.69163855873949132 ) ) ;
#10022 = CARTESIAN_POINT ( 'NONE',  ( -30.99614452189004155, 33.97742542711323921, 0.0005215828242728561687 ) ) ;
#10023 =( NAMED_UNIT ( * ) SI_UNIT ( $, .STERADIAN. ) SOLID_ANGLE_UNIT ( ) );
#10024 = ORIENTED_EDGE ( 'NONE', *, *, #5414, .T. ) ;
#10025 = ADVANCED_FACE ( 'NONE', ( #2111 ), #2239, .F. ) ;
#10026 = DIRECTION ( 'NONE',  ( 1.000000000000000000, 0.000000000000000000, 0.000000000000000000 ) ) ;
#10027 = AXIS2_PLACEMENT_3D ( 'NONE', #673, #11450, #6268 ) ;
#10028 = CARTESIAN_POINT ( 'NONE',  ( -12.43046839200774656, 54.98819421727549184, 0.003555045980302951828 ) ) ;
#10029 = ORIENTED_EDGE ( 'NONE', *, *, #439, .T. ) ;
#10030 = CARTESIAN_POINT ( 'NONE',  ( -29.03064367431483817, 36.00003416271029266, 8.986251614625855311 ) ) ;
#10031 = CARTESIAN_POINT ( 'NONE',  ( -32.40407992077046373, 34.08317752212569474, 2.058454929014103651 ) ) ;
#10032 = CYLINDRICAL_SURFACE ( 'NONE', #4911, 1.500000000000000000 ) ;
#10033 = CARTESIAN_POINT ( 'NONE',  ( 0.000000000000000000, 50.52094453300079380, 17.04557674096337649 ) ) ;
#10034 = DIRECTION ( 'NONE',  ( -1.000000000000000000, -0.000000000000000000, -0.000000000000000000 ) ) ;
#10035 = FACE_OUTER_BOUND ( 'NONE', #1214, .T. ) ;
#10036 = ADVANCED_FACE ( 'NONE', ( #191 ), #5725, .T. ) ;
#10037 = ORIENTED_EDGE ( 'NONE', *, *, #4441, .T. ) ;
#10038 = PLANE ( 'NONE',  #11095 ) ;
#10039 = CARTESIAN_POINT ( 'NONE',  ( -55.87153088905797915, 55.00233510441087503, 0.001258675581659554621 ) ) ;
#10040 = CARTESIAN_POINT ( 'NONE',  ( -37.62597467746413571, 53.39124767624571888, -4.745502624100200073 ) ) ;
#10041 = CARTESIAN_POINT ( 'NONE',  ( -77.56250000000007105, 37.32233047033638229, 17.67766952966362837 ) ) ;
#10042 = DIRECTION ( 'NONE',  ( -1.000000000000000000, 0.000000000000000000, 0.000000000000000000 ) ) ;
#10043 = ORIENTED_EDGE ( 'NONE', *, *, #6551, .T. ) ;
#10044 = DIRECTION ( 'NONE',  ( -0.000000000000000000, -0.000000000000000000, -1.000000000000000000 ) ) ;
#10045 = CARTESIAN_POINT ( 'NONE',  ( 39.99999999999999289, 55.00000000000000000, 0.000000000000000000 ) ) ;
#10046 = CARTESIAN_POINT ( 'NONE',  ( -78.00000000000001421, 46.51471862576140381, -9.985278002320759683 ) ) ;
#10047 = CARTESIAN_POINT ( 'NONE',  ( -80.00000000000002842, 46.51471862576140381, 8.485284746156354529 ) ) ;
#10048 = CARTESIAN_POINT ( 'NONE',  ( -75.87500000204839523, 65.69163855873949842, 25.81189881250000440 ) ) ;
#10049 = VECTOR ( 'NONE', #7176, 1000.000000000000000 ) ;
#10050 = ORIENTED_EDGE ( 'NONE', *, *, #1881, .F. ) ;
#10051 = CARTESIAN_POINT ( 'NONE',  ( -74.28125000204839523, 73.25176868561975141, 18.25176868561974075 ) ) ;
#10052 = ORIENTED_EDGE ( 'NONE', *, *, #2024, .F. ) ;
#10053 = CARTESIAN_POINT ( 'NONE',  ( 52.99999999999999289, 55.00000000000000000, 2.999999999999999112 ) ) ;
#10054 = CARTESIAN_POINT ( 'NONE',  ( -16.36967209184480865, 65.37984753263212667, 9.407486617481991331 ) ) ;
#10055 = CIRCLE ( 'NONE', #6075, 1.500000000000001332 ) ;
#10056 = DIRECTION ( 'NONE',  ( 0.000000000000000000, 0.000000000000000000, -1.000000000000000000 ) ) ;
#10057 = CARTESIAN_POINT ( 'NONE',  ( -74.99999999999997158, 67.69301918158085130, -22.29621844334601377 ) ) ;
#10058 = AXIS2_PLACEMENT_3D ( 'NONE', #9368, #5070, #258 ) ;
#10059 = CARTESIAN_POINT ( 'NONE',  ( -78.21875000000004263, 79.99999999999992895, -10.35533905932734910 ) ) ;
#10060 = EDGE_LOOP ( 'NONE', ( #571, #6446 ) ) ;
#10061 = AXIS2_PLACEMENT_3D ( 'NONE', #9757, #5395, #11730 ) ;
#10062 = CARTESIAN_POINT ( 'NONE',  ( 9.999999999999994671, 0.000000000000000000, 10.00000000000000000 ) ) ;
#10063 = CARTESIAN_POINT ( 'NONE',  ( -73.15625000204839523, 73.25176868561975141, -18.25176868561974430 ) ) ;
#10064 = FACE_OUTER_BOUND ( 'NONE', #10120, .T. ) ;
#10065 = CARTESIAN_POINT ( 'NONE',  ( -54.49661136968474295, 55.00298157538451704, 0.003101384249735006544 ) ) ;
#10066 = CARTESIAN_POINT ( 'NONE',  ( -21.53847754367192380, 76.85212920633969702, -2.572070869066138687 ) ) ;
#10067 = VECTOR ( 'NONE', #9266, 1000.000000000000000 ) ;
#10068 = CARTESIAN_POINT ( 'NONE',  ( 14.99999999999999645, -30.00000000000000000, 10.00000000000000000 ) ) ;
#10069 = AXIS2_PLACEMENT_3D ( 'NONE', #2992, #2023, #9397 ) ;
#10070 = ORIENTED_EDGE ( 'NONE', *, *, #6469, .T. ) ;
#10071 = CARTESIAN_POINT ( 'NONE',  ( -74.37500000409677625, 55.00000000000000000, -24.99999999999999645 ) ) ;
#10072 = EDGE_LOOP ( 'NONE', ( #4989, #704, #4235, #8523 ) ) ;
#10073 = CARTESIAN_POINT ( 'NONE',  ( -68.15132479584509895, 34.52429035776697930, 5.502002828716508809 ) ) ;
#10074 = CARTESIAN_POINT ( 'NONE',  ( -77.93750000204838102, 44.30836144126050158, -25.81189881249999374 ) ) ;
#10075 = EDGE_CURVE ( 'NONE', #8154, #9967, #11087, .T. ) ;
#10076 = AXIS2_PLACEMENT_3D ( 'NONE', #4454, #4506, #958 ) ;
#10077 = ORIENTED_EDGE ( 'NONE', *, *, #7659, .F. ) ;
#10078 = CARTESIAN_POINT ( 'NONE',  ( -73.15625000204838102, 80.81189881250000440, -1.580522963032174394E-15 ) ) ;
#10079 = CARTESIAN_POINT ( 'NONE',  ( -9.391823749396904120, 73.59702374900430755, -9.931971109272440756 ) ) ;
#10080 = SURFACE_STYLE_USAGE ( .BOTH. , #3869 ) ;
#10081 = CARTESIAN_POINT ( 'NONE',  ( -68.34104732181945963, 33.99448141944315438, 0.006743540747239065887 ) ) ;
#10082 = VERTEX_POINT ( 'NONE', #4694 ) ;
#10083 = CARTESIAN_POINT ( 'NONE',  ( -5.371237946277282127, 54.66875656801337158, -4.999992488715903960 ) ) ;
#10084 = DIRECTION ( 'NONE',  ( 0.000000000000000000, 0.000000000000000000, 1.000000000000000000 ) ) ;
#10085 = CONICAL_SURFACE ( 'NONE', #7439, 2.500000000000000000, 0.9599310885968755924 ) ;
#10086 = ORIENTED_EDGE ( 'NONE', *, *, #11568, .F. ) ;
#10087 = CARTESIAN_POINT ( 'NONE',  ( -42.73741365937004844, 61.10231602703586873, -20.11119678530976884 ) ) ;
#10088 = CARTESIAN_POINT ( 'NONE',  ( -19.00387657603030078, 69.86840152515847535, 14.86901714484747750 ) ) ;
#10089 = CARTESIAN_POINT ( 'NONE',  ( -4.999999999999999112, -0.4878135028931870898, 5.217722955086490089E-16 ) ) ;
#10090 = CARTESIAN_POINT ( 'NONE',  ( -30.23830917210572267, 50.00000000000000711, 1.120793995806890209E-14 ) ) ;
#10091 = LINE ( 'NONE', #28, #4403 ) ;
#10092 = DIRECTION ( 'NONE',  ( -0.000000000000000000, -0.000000000000000000, 1.000000000000000000 ) ) ;
#10093 = ADVANCED_FACE ( 'NONE', ( #6749 ), #5841, .T. ) ;
#10094 = ORIENTED_EDGE ( 'NONE', *, *, #1408, .F. ) ;
#10095 = DIRECTION ( 'NONE',  ( -0.000000000000000000, -1.000000000000000000, -0.000000000000000000 ) ) ;
#10096 = CARTESIAN_POINT ( 'NONE',  ( -37.09269367797786998, 54.98551036657900681, -0.007796657494142412992 ) ) ;
#10097 = CARTESIAN_POINT ( 'NONE',  ( -30.23830917210572267, 50.00000000000000711, 1.120793995806890209E-14 ) ) ;
#10098 = FACE_OUTER_BOUND ( 'NONE', #1939, .T. ) ;
#10099 = DIRECTION ( 'NONE',  ( -0.000000000000000000, -1.000000000000000000, -0.000000000000000000 ) ) ;
#10100 = ADVANCED_FACE ( 'NONE', ( #1212 ), #4756, .T. ) ;
#10101 = CIRCLE ( 'NONE', #159, 4.000000000000003553 ) ;
#10102 = ORIENTED_EDGE ( 'NONE', *, *, #6255, .F. ) ;
#10103 = CARTESIAN_POINT ( 'NONE',  ( 4.881307793505825110, 34.60946683332392126, -5.106800360247272685 ) ) ;
#10104 = DIRECTION ( 'NONE',  ( 1.000000000000000000, 6.033820786006286457E-17, 0.000000000000000000 ) ) ;
#10105 = FACE_OUTER_BOUND ( 'NONE', #8420, .T. ) ;
#10106 = CARTESIAN_POINT ( 'NONE',  ( -23.15625510892966687, 78.18806447604573862, -9.352364031898828145 ) ) ;
#10107 = CARTESIAN_POINT ( 'NONE',  ( -75.31250000204839523, 29.18810118750000626, -10.69163855873949309 ) ) ;
#10108 = ORIENTED_EDGE ( 'NONE', *, *, #8410, .F. ) ;
#10109 = CARTESIAN_POINT ( 'NONE',  ( -78.12500000204838102, 29.18810118750000626, -10.69163855873949309 ) ) ;
#10110 = CIRCLE ( 'NONE', #3044, 1.500000000000001332 ) ;
#10111 = ORIENTED_EDGE ( 'NONE', *, *, #4925, .F. ) ;
#10112 = CARTESIAN_POINT ( 'NONE',  ( 22.61952844766377169, 77.73902299693440909, 10.39627090682546928 ) ) ;
#10113 = AXIS2_PLACEMENT_3D ( 'NONE', #6766, #6705, #3932 ) ;
#10114 = EDGE_CURVE ( 'NONE', #3861, #3881, #514, .T. ) ;
#10115 = CARTESIAN_POINT ( 'NONE',  ( -17.54480031048505495, 63.35260169467658642, 11.26165491496548832 ) ) ;
#10116 = CARTESIAN_POINT ( 'NONE',  ( -75.40625000204839523, 36.74823131438026280, 18.25176868561974786 ) ) ;
#10117 = CARTESIAN_POINT ( 'NONE',  ( -74.99999999999998579, 68.14082849008082121, -22.02527069007740934 ) ) ;
#10118 = DIRECTION ( 'NONE',  ( -1.000000000000000000, -0.000000000000000000, -0.000000000000000000 ) ) ;
#10119 = AXIS2_PLACEMENT_3D ( 'NONE', #7149, #3356, #2584 ) ;
#10120 = EDGE_LOOP ( 'NONE', ( #8856, #6095, #4414, #11463 ) ) ;
#10121 = CARTESIAN_POINT ( 'NONE',  ( -79.53125000000000000, 80.00000000000001421, 10.35533905932737397 ) ) ;
#10122 = CARTESIAN_POINT ( 'NONE',  ( -77.75000000409677625, 30.00000000000000355, 4.592425496802573578E-15 ) ) ;
#10123 = DIRECTION ( 'NONE',  ( 0.000000000000000000, 0.000000000000000000, 1.000000000000000000 ) ) ;
#10124 = CARTESIAN_POINT ( 'NONE',  ( -60.33684501428881930, 55.00322620591916944, -0.003862519133706141233 ) ) ;
#10125 = PRODUCT_CONTEXT ( 'NONE', #1863, 'mechanical' ) ;
#10126 = CIRCLE ( 'NONE', #4025, 1.500000000000001332 ) ;
#10127 = CARTESIAN_POINT ( 'NONE',  ( 2.400054171417768487E-15, 64.99605696851786263, -19.59792961213366169 ) ) ;
#10128 = LINE ( 'NONE', #4754, #109 ) ;
#10129 = VERTEX_POINT ( 'NONE', #9298 ) ;
#10130 = CARTESIAN_POINT ( 'NONE',  ( 11.37836091825973561, 51.23382177081494149, 3.305048827278960211 ) ) ;
#10131 = DIRECTION ( 'NONE',  ( 1.000000000000000000, 6.033820786006286457E-17, -0.000000000000000000 ) ) ;
#10132 = ORIENTED_EDGE ( 'NONE', *, *, #10975, .T. ) ;
#10133 = CARTESIAN_POINT ( 'NONE',  ( -1.855729112296511385, 44.43418165317581980, -18.33336562707187412 ) ) ;
#10134 = AXIS2_PLACEMENT_3D ( 'NONE', #8001, #7114, #7056 ) ;
#10135 = CARTESIAN_POINT ( 'NONE',  ( -77.00000000204838102, 44.30836144126053000, 25.81189881250000795 ) ) ;
#10136 = ORIENTED_EDGE ( 'NONE', *, *, #5408, .F. ) ;
#10137 = DIRECTION ( 'NONE',  ( 1.000000000000000000, 6.033820786006286457E-17, 0.000000000000000000 ) ) ;
#10138 = CARTESIAN_POINT ( 'NONE',  ( 4.003855478097921861, 35.57747403031575573, -8.044509115018048107 ) ) ;
#10139 = VECTOR ( 'NONE', #29, 1000.000000000000000 ) ;
#10140 =( NAMED_UNIT ( * ) PLANE_ANGLE_UNIT ( ) SI_UNIT ( $, .RADIAN. ) );
#10141 = CARTESIAN_POINT ( 'NONE',  ( -40.33720992201957500, 55.00042869323097960, -21.02810349118288258 ) ) ;
#10142 = ORIENTED_EDGE ( 'NONE', *, *, #4890, .F. ) ;
#10143 = DIRECTION ( 'NONE',  ( -1.000000000000000000, 0.000000000000000000, 0.000000000000000000 ) ) ;
#10144 = CIRCLE ( 'NONE', #7113, 22.00000000000000000 ) ;
#10145 = CARTESIAN_POINT ( 'NONE',  ( 2.500000000000000000, 0.000000000000000000, -1.239675197676287643 ) ) ;
#10146 = CARTESIAN_POINT ( 'NONE',  ( -77.75000000000000000, 55.00000000000000000, 24.99999999999999645 ) ) ;
#10147 = ORIENTED_EDGE ( 'NONE', *, *, #9664, .T. ) ;
#10148 = CARTESIAN_POINT ( 'NONE',  ( -17.36397700743563632, 70.57318608196271725, 14.11478994354440530 ) ) ;
#10149 = CIRCLE ( 'NONE', #9389, 5.048155585660824229 ) ;
#10150 = AXIS2_PLACEMENT_3D ( 'NONE', #4021, #6732, #11188 ) ;
#10151 = CARTESIAN_POINT ( 'NONE',  ( -55.73751408985167899, 71.24607175163586703, 13.33484869932101269 ) ) ;
#10152 = CARTESIAN_POINT ( 'NONE',  ( 4.999999999999999112, -2.417244626924489825, -0.3110470720778663600 ) ) ;
#10153 =( NAMED_UNIT ( * ) SI_UNIT ( $, .STERADIAN. ) SOLID_ANGLE_UNIT ( ) );
#10154 = CARTESIAN_POINT ( 'NONE',  ( -78.00000000000002842, 54.99999999999998579, 9.985284746156354529 ) ) ;
#10155 = CARTESIAN_POINT ( 'NONE',  ( -78.00000000000001421, 63.48528137423857487, -1.499996628082204797 ) ) ;
#10156 = ADVANCED_FACE ( 'NONE', ( #3017 ), #1091, .F. ) ;
#10157 = EDGE_CURVE ( 'NONE', #7832, #6451, #1271, .T. ) ;
#10158 = ORIENTED_EDGE ( 'NONE', *, *, #11168, .F. ) ;
#10159 = LINE ( 'NONE', #11723, #3476 ) ;
#10160 = CARTESIAN_POINT ( 'NONE',  ( -26.24059676141881781, 55.00778171745486134, -0.01448394145446873539 ) ) ;
#10161 = FACE_OUTER_BOUND ( 'NONE', #5501, .T. ) ;
#10162 = VECTOR ( 'NONE', #841, 1000.000000000000000 ) ;
#10163 = CARTESIAN_POINT ( 'NONE',  ( -80.00000000000001421, 59.24264068711927678, -2.742637315201482462 ) ) ;
#10164 = PRODUCT_DEFINITION_SHAPE ( 'NONE', 'NONE',  #11857 ) ;
#10165 = CARTESIAN_POINT ( 'NONE',  ( 53.00000000000000000, 2.835895769422954721E-15, 0.000000000000000000 ) ) ;
#10166 = CARTESIAN_POINT ( 'NONE',  ( -56.96367441743876725, 64.41719779848563121, 10.39011149079907526 ) ) ;
#10167 = EDGE_LOOP ( 'NONE', ( #9950, #3214 ) ) ;
#10168 = CARTESIAN_POINT ( 'NONE',  ( 2.826857198123298165, 37.44742646213195769, -11.71858918393001225 ) ) ;
#10169 = CARTESIAN_POINT ( 'NONE',  ( -78.00000000000001421, 50.75735931288069480, -11.22791868944003824 ) ) ;
#10170 = LINE ( 'NONE', #11786, #195 ) ;
#10171 = CARTESIAN_POINT ( 'NONE',  ( -80.00000000000001421, 54.99999999999998579, -9.985278002320759683 ) ) ;
#10172 = CARTESIAN_POINT ( 'NONE',  ( -71.53052369147286527, 77.35376373433385311, 12.90594309674112949 ) ) ;
#10173 = CARTESIAN_POINT ( 'NONE',  ( -76.34375000204839523, 73.25176868561975141, -18.25176868561974430 ) ) ;
#10174 = EDGE_CURVE ( 'NONE', #8848, #10918, #9889, .T. ) ;
#10175 = EDGE_LOOP ( 'NONE', ( #152, #11059 ) ) ;
#10176 = ADVANCED_FACE ( 'NONE', ( #6802 ), #1149, .F. ) ;
#10177 = EDGE_CURVE ( 'NONE', #7683, #322, #2439, .T. ) ;
#10178 = DIRECTION ( 'NONE',  ( 1.000000000000000000, 6.033820786006286457E-17, -0.000000000000000000 ) ) ;
#10179 = VERTEX_POINT ( 'NONE', #3313 ) ;
#10180 = CARTESIAN_POINT ( 'NONE',  ( 2.782474192756827142E-15, 65.42943686846950868, -22.72062601704910634 ) ) ;
#10181 = CARTESIAN_POINT ( 'NONE',  ( -55.73773073934312805, 61.61875917375134293, 12.39151048960789048 ) ) ;
#10182 = CARTESIAN_POINT ( 'NONE',  ( -78.96875000204839523, 73.25176868561975141, 18.25176868561974075 ) ) ;
#10183 = CARTESIAN_POINT ( 'NONE',  ( -75.00000000000000000, 78.87322666461865595, 7.729222434168494971 ) ) ;
#10184 = EDGE_CURVE ( 'NONE', #10529, #2054, #10201, .T. ) ;
#10185 = EDGE_CURVE ( 'NONE', #9767, #1442, #7331, .T. ) ;
#10186 = FACE_OUTER_BOUND ( 'NONE', #11507, .T. ) ;
#10187 = EDGE_LOOP ( 'NONE', ( #9400, #10199, #8232, #5554 ) ) ;
#10188 = EDGE_CURVE ( 'NONE', #1033, #6241, #1857, .T. ) ;
#10189 = CARTESIAN_POINT ( 'NONE',  ( 2.500000000000000000, 0.000000000000000000, -6.099999999999999645 ) ) ;
#10190 = CARTESIAN_POINT ( 'NONE',  ( -77.28125000409677625, 65.35533905932737753, -24.99999999999999645 ) ) ;
#10191 = DIRECTION ( 'NONE',  ( -0.000000000000000000, -1.000000000000000000, -0.000000000000000000 ) ) ;
#10192 = CARTESIAN_POINT ( 'NONE',  ( -15.00000000000000000, 55.00000000000000000, -20.00000000000000000 ) ) ;
#10193 = CARTESIAN_POINT ( 'NONE',  ( -0.7765809050102786548, 53.15807774253367057, -6.841262966262681822 ) ) ;
#10194 = CARTESIAN_POINT ( 'NONE',  ( -21.48451911196086073, 76.80686963222734676, -2.931110701500045046 ) ) ;
#10195 = CARTESIAN_POINT ( 'NONE',  ( -5.000000000000000000, 2.886751345948134428, -5.653418012614792154 ) ) ;
#10196 = VERTEX_POINT ( 'NONE', #6315 ) ;
#10197 = DIRECTION ( 'NONE',  ( -1.000000000000000000, -6.033820786006286457E-17, 0.000000000000000000 ) ) ;
#10198 = CYLINDRICAL_SURFACE ( 'NONE', #5180, 4.999999999999984013 ) ;
#10199 = ORIENTED_EDGE ( 'NONE', *, *, #11357, .T. ) ;
#10200 = CARTESIAN_POINT ( 'NONE',  ( 9.810937555461070048, 42.10554236623130464, 16.77741859935663626 ) ) ;
#10201 = B_SPLINE_CURVE_WITH_KNOTS ( 'NONE', 3,
 ( #5060, #6865, #1572, #3252, #11505, #6980, #7985, #7750, #11563, #10602, #1339, #611, #2408, #7931, #6081, #4092, #10489, #11384, #9544, #4212, #5970, #8708, #1398, #9715, #5237, #9774, #10554, #1511, #11624, #492, #2354, #6023, #8884, #8828, #7811, #9658, #664, #2295, #5175, #4334, #5001, #4273, #8652, #5901, #3365, #3425, #9607, #1456, #431, #3192, #7041, #2472, #10430, #4147, #5118, #11442, #6922, #8767, #547, #778, #9057, #1624, #9948, #10842 ),
 .UNSPECIFIED., .F., .F.,
 ( 4, 2, 2, 2, 2, 2, 2, 2, 2, 2, 2, 2, 2, 2, 2, 2, 2, 2, 2, 2, 2, 2, 2, 2, 2, 2, 2, 2, 2, 2, 2, 4 ),
 ( 0.1342163981613174739, 0.1363961341890387868, 0.1385758702167600998, 0.1407556062444813849, 0.1429353422722026978, 0.1472948143276453237, 0.1494745503553666088, 0.1516542863830879218, 0.1560137584385305476, 0.1603732304939732012, 0.1614630985078338576, 0.1625529665216945141, 0.1647327025494158825, 0.1669124385771372232, 0.1680023065909978797, 0.1690921746048585639, 0.1712719106325799046, 0.1734516466603012175, 0.1756313826880225581, 0.1778111187157438988, 0.1821705907711865802, 0.1843503267989079208, 0.1865300628266292615, 0.1908895348820719151, 0.1930692709097932558, 0.1952490069375145687, 0.1974287429652359094, 0.1985186109790965658, 0.1996084789929572501, 0.2017882150206785630, 0.2028780830345392472, 0.2039679510483999314 ),
 .UNSPECIFIED. ) ;
#10202 = CARTESIAN_POINT ( 'NONE',  ( -74.09375000204839523, 36.74823131438026280, 18.25176868561974786 ) ) ;
#10203 = CYLINDRICAL_SURFACE ( 'NONE', #1381, 1.500000000000000000 ) ;
#10204 = CARTESIAN_POINT ( 'NONE',  ( -15.82693394478133797, 72.53700911420227726, 11.72543866452437733 ) ) ;
#10205 = FILL_AREA_STYLE ('',( #2909 ) ) ;
#10206 = DIRECTION ( 'NONE',  ( 1.000000000000000000, 6.033820786006286457E-17, 0.000000000000000000 ) ) ;
#10207 = ORIENTED_EDGE ( 'NONE', *, *, #10800, .F. ) ;
#10208 = DIRECTION ( 'NONE',  ( -0.000000000000000000, -0.000000000000000000, -1.000000000000000000 ) ) ;
#10209 = CARTESIAN_POINT ( 'NONE',  ( -4.208370785906845768, 53.70404148446576897, -4.840060944352733152 ) ) ;
#10210 = CARTESIAN_POINT ( 'NONE',  ( 0.000000000000000000, 50.52094453300079380, 0.000000000000000000 ) ) ;
#10211 = ORIENTED_EDGE ( 'NONE', *, *, #8355, .T. ) ;
#10212 = CARTESIAN_POINT ( 'NONE',  ( -28.16026721702189306, 37.45568712642866416, 11.71507272220211071 ) ) ;
#10213 = CARTESIAN_POINT ( 'NONE',  ( 21.87131398367523616, 69.01805473306414740, 1.834616117294233240 ) ) ;
#10214 = CARTESIAN_POINT ( 'NONE',  ( -73.53125000409677625, 44.64466094067245905, 24.99999999999983658 ) ) ;
#10215 = FILL_AREA_STYLE ('',( #7597 ) ) ;
#10216 = CARTESIAN_POINT ( 'NONE',  ( -78.00000000000002842, 42.27207793864211283, -2.742637315201478909 ) ) ;
#10217 = FACE_OUTER_BOUND ( 'NONE', #715, .T. ) ;
#10218 = ORIENTED_EDGE ( 'NONE', *, *, #8135, .T. ) ;
#10219 = EDGE_CURVE ( 'NONE', #9312, #8530, #4782, .T. ) ;
#10220 = CARTESIAN_POINT ( 'NONE',  ( -76.90625000000000000, 65.35533905932737753, -24.99999999999999645 ) ) ;
#10221 = CARTESIAN_POINT ( 'NONE',  ( -33.42366184627161374, 55.00651688198467326, 0.0004154897275390965193 ) ) ;
#10222 = CARTESIAN_POINT ( 'NONE',  ( -49.29517856930504394, 60.00000000000064659, 0.3319123253646104055 ) ) ;
#10223 = CARTESIAN_POINT ( 'NONE',  ( 9.999999999999994671, -30.00000000000000000, 10.00000000000000000 ) ) ;
#10224 = CARTESIAN_POINT ( 'NONE',  ( -78.40625000409677625, 80.00000000000001421, 10.35533905932737397 ) ) ;
#10225 = CARTESIAN_POINT ( 'NONE',  ( 4.833109902090660270, 48.10506029203823175, 1.369963280143046136 ) ) ;
#10226 = EDGE_LOOP ( 'NONE', ( #6202, #1070, #404, #7524 ) ) ;
#10227 = DIRECTION ( 'NONE',  ( 0.000000000000000000, 1.000000000000000000, 0.000000000000000000 ) ) ;
#10228 = FACE_OUTER_BOUND ( 'NONE', #8544, .T. ) ;
#10229 = DIRECTION ( 'NONE',  ( 1.000000000000000000, 0.000000000000000000, 0.000000000000000000 ) ) ;
#10230 = CARTESIAN_POINT ( 'NONE',  ( -79.25000000204839523, 65.69163855873948421, -25.81189881250000084 ) ) ;
#10231 = CARTESIAN_POINT ( 'NONE',  ( -2.993446321628384865, 65.73059443587099793, -22.58010246442618296 ) ) ;
#10232 = CARTESIAN_POINT ( 'NONE',  ( -72.87500000204839523, 65.69163855873949842, 25.81189881250000440 ) ) ;
#10233 = VERTEX_POINT ( 'NONE', #8276 ) ;
#10234 = CARTESIAN_POINT ( 'NONE',  ( -78.68750000409679046, 72.67766952966368876, -17.67766952966368876 ) ) ;
#10235 = ORIENTED_EDGE ( 'NONE', *, *, #5148, .F. ) ;
#10236 = CARTESIAN_POINT ( 'NONE',  ( 14.31283626472151482, 71.29068060248663130, -18.97189842681568805 ) ) ;
#10237 = CARTESIAN_POINT ( 'NONE',  ( 21.85574933723554736, 73.37275400661043534, 10.58193396047185075 ) ) ;
#10238 = CARTESIAN_POINT ( 'NONE',  ( -78.00000000000001421, 67.72792206135787296, 2.742644059037073312 ) ) ;
#10239 = CARTESIAN_POINT ( 'NONE',  ( -74.99999999999998579, 77.92805329443815765, -10.94505072500436604 ) ) ;
#10240 = LINE ( 'NONE', #240, #903 ) ;
#10241 = ORIENTED_EDGE ( 'NONE', *, *, #10800, .T. ) ;
#10242 = AXIS2_PLACEMENT_3D ( 'NONE', #1708, #4416, #5257 ) ;
#10243 = DIRECTION ( 'NONE',  ( 0.000000000000000000, 0.000000000000000000, 1.000000000000000000 ) ) ;
#10244 = CARTESIAN_POINT ( 'NONE',  ( -74.09375000409676204, 80.00000000000001421, -10.35533905932737753 ) ) ;
#10245 = CYLINDRICAL_SURFACE ( 'NONE', #11290, 2.500000000000000000 ) ;
#10246 = FACE_BOUND ( 'NONE', #6804, .T. ) ;
#10247 = ADVANCED_FACE ( 'NONE', ( #9835 ), #3606, .T. ) ;
#10248 = CARTESIAN_POINT ( 'NONE',  ( -16.33319360682722632, 59.95766673739793617, 4.958029769595817982 ) ) ;
#10249 = DIRECTION ( 'NONE',  ( 6.033820786006286457E-17, -1.000000000000000000, 0.000000000000000000 ) ) ;
#10250 = VECTOR ( 'NONE', #3090, 1000.000000000000000 ) ;
#10251 = CARTESIAN_POINT ( 'NONE',  ( -78.00000000000001421, 42.27207793864211283, -11.22791868944003824 ) ) ;
#10252 = ORIENTED_EDGE ( 'NONE', *, *, #8663, .T. ) ;
#10253 = DIRECTION ( 'NONE',  ( 0.000000000000000000, 0.000000000000000000, 1.000000000000000000 ) ) ;
#10254 = AXIS2_PLACEMENT_3D ( 'NONE', #2169, #1930, #8285 ) ;
#10255 = LINE ( 'NONE', #10, #4996 ) ;
#10256 = ADVANCED_FACE ( 'NONE', ( #2650 ), #4622, .F. ) ;
#10257 = ORIENTED_EDGE ( 'NONE', *, *, #206, .T. ) ;
#10258 = CARTESIAN_POINT ( 'NONE',  ( -15.85565286160008469, 75.43490621471428881, 5.492246195135631837 ) ) ;
#10259 = CARTESIAN_POINT ( 'NONE',  ( -71.46875000204838102, 80.81189881250000440, -1.580522963032174394E-15 ) ) ;
#10260 = DIRECTION ( 'NONE',  ( -0.000000000000000000, -0.000000000000000000, -1.000000000000000000 ) ) ;
#10261 = CARTESIAN_POINT ( 'NONE',  ( -55.50627899214600092, 66.73177265193905328, 17.54361557889675893 ) ) ;
#10262 = AXIS2_PLACEMENT_3D ( 'NONE', #5951, #6851, #5159 ) ;
#10263 = SURFACE_STYLE_USAGE ( .BOTH. , #10326 ) ;
#10264 = AXIS2_PLACEMENT_3D ( 'NONE', #8445, #8263, #3765 ) ;
#10265 = CARTESIAN_POINT ( 'NONE',  ( 19.99999999999996803, -63.00000000000000000, -5.000000000000000000 ) ) ;
#10266 = ORIENTED_EDGE ( 'NONE', *, *, #1168, .T. ) ;
#10267 = CARTESIAN_POINT ( 'NONE',  ( -72.68750000204839523, 65.69163855873949842, 25.81189881250000084 ) ) ;
#10268 = LINE ( 'NONE', #10145, #556 ) ;
#10269 = CARTESIAN_POINT ( 'NONE',  ( -78.03125000000002842, 79.99999999999992895, 10.35533905932734378 ) ) ;
#10270 = ORIENTED_EDGE ( 'NONE', *, *, #6770, .T. ) ;
#10271 = CARTESIAN_POINT ( 'NONE',  ( -30.21475903739694857, 34.60120891540925925, 5.109855906315051044 ) ) ;
#10272 = CARTESIAN_POINT ( 'NONE',  ( -54.00383531698385298, 74.42670172875287449, 8.047314657126378279 ) ) ;
#10273 = SURFACE_STYLE_USAGE ( .BOTH. , #6641 ) ;
#10274 = CARTESIAN_POINT ( 'NONE',  ( -75.87500000409677625, 55.00000000000000000, -24.99999999999999645 ) ) ;
#10275 = VECTOR ( 'NONE', #1851, 1000.000000000000000 ) ;
#10276 = CARTESIAN_POINT ( 'NONE',  ( -16.65533121350868839, 59.83994479200593020, 1.296523861810935374 ) ) ;
#10277 = CARTESIAN_POINT ( 'NONE',  ( -75.21875000000007105, 79.99999999999990052, -10.35533905932733312 ) ) ;
#10278 = VERTEX_POINT ( 'NONE', #1745 ) ;
#10279 = EDGE_CURVE ( 'NONE', #9873, #10795, #11743, .T. ) ;
#10280 = FACE_OUTER_BOUND ( 'NONE', #11678, .T. ) ;
#10281 = CARTESIAN_POINT ( 'NONE',  ( -74.99999999999998579, 55.08591585515510047, -25.82567655465456724 ) ) ;
#10282 = APPLICATION_CONTEXT ( 'automotive_design' ) ;
#10283 = DIRECTION ( 'NONE',  ( -0.000000000000000000, -0.000000000000000000, -1.000000000000000000 ) ) ;
#10284 = CARTESIAN_POINT ( 'NONE',  ( -77.00000000000000000, 55.00000000000000000, -24.99999999999999645 ) ) ;
#10285 = VECTOR ( 'NONE', #4442, 1000.000000000000000 ) ;
#10286 = PLANE ( 'NONE',  #5486 ) ;
#10287 = CARTESIAN_POINT ( 'NONE',  ( -56.66487171987550653, 64.91036822740932166, 9.909685932910122119 ) ) ;
#10288 = ORIENTED_EDGE ( 'NONE', *, *, #9081, .F. ) ;
#10289 = CARTESIAN_POINT ( 'NONE',  ( 10.18903847268274276, 38.19250115101311849, 12.92455934260550521 ) ) ;
#10290 = CARTESIAN_POINT ( 'NONE',  ( -78.00000000000002842, 50.75735931288069480, 12.72792543327563131 ) ) ;
#10291 = FACE_OUTER_BOUND ( 'NONE', #5779, .T. ) ;
#10292 = CARTESIAN_POINT ( 'NONE',  ( -80.00000000000001421, 63.48528137423857487, 9.985284746156350977 ) ) ;
#10293 = CARTESIAN_POINT ( 'NONE',  ( -23.67934118466866877, 78.62819164648935555, 8.208188635330966321 ) ) ;
#10294 = CARTESIAN_POINT ( 'NONE',  ( -72.96875000204838102, 73.25176868561975141, 18.25176868561974075 ) ) ;
#10295 = ORIENTED_EDGE ( 'NONE', *, *, #2800, .F. ) ;
#10296 = CARTESIAN_POINT ( 'NONE',  ( -77.56250000409679046, 37.32233047033631124, -17.67766952966368166 ) ) ;
#10297 = ORIENTED_EDGE ( 'NONE', *, *, #5370, .T. ) ;
#10298 =( LENGTH_UNIT ( ) NAMED_UNIT ( * ) SI_UNIT ( .MILLI., .METRE. ) );
#10299 = CARTESIAN_POINT ( 'NONE',  ( -33.79373960940952770, 42.74365976533915301, -7.058510872263445535 ) ) ;
#10300 = EDGE_CURVE ( 'NONE', #5239, #10429, #9522, .T. ) ;
#10301 = CARTESIAN_POINT ( 'NONE',  ( -71.53052369147287948, 77.35376373433385311, 12.90594309674112772 ) ) ;
#10302 = CARTESIAN_POINT ( 'NONE',  ( -75.00000000000000000, 71.47984153822721964, -19.58526305464525308 ) ) ;
#10303 = CARTESIAN_POINT ( 'NONE',  ( -78.00000000000001421, 59.24264068711927678, 2.742644059037073312 ) ) ;
#10304 = ORIENTED_EDGE ( 'NONE', *, *, #9294, .T. ) ;
#10305 = CARTESIAN_POINT ( 'NONE',  ( -74.46875000000008527, 30.00000000000014921, 10.35533905932733489 ) ) ;
#10306 = CARTESIAN_POINT ( 'NONE',  ( -74.28125000409676204, 65.35533905932737753, -24.99999999999999645 ) ) ;
#10307 = VECTOR ( 'NONE', #11649, 1000.000000000000000 ) ;
#10308 = FACE_OUTER_BOUND ( 'NONE', #4570, .T. ) ;
#10309 = EDGE_CURVE ( 'NONE', #2213, #66, #7100, .T. ) ;
#10310 = CARTESIAN_POINT ( 'NONE',  ( 20.22335381278353594, 59.31970004319295953, 5.615686161229384687 ) ) ;
#10311 = CARTESIAN_POINT ( 'NONE',  ( -72.96875000000007105, 30.00000000000015277, 10.35533905932733312 ) ) ;
#10312 = CONICAL_SURFACE ( 'NONE', #5162, 5.000000000000000888, 1.047197551196596299 ) ;
#10313 = CARTESIAN_POINT ( 'NONE',  ( -80.00000000000002842, 54.99999999999998579, 8.485284746156354529 ) ) ;
#10314 = CIRCLE ( 'NONE', #172, 1.500000000000001332 ) ;
#10315 = ORIENTED_EDGE ( 'NONE', *, *, #10174, .T. ) ;
#10316 = CARTESIAN_POINT ( 'NONE',  ( 36.99999999999999289, 59.99999999999998579, 0.000000000000000000 ) ) ;
#10317 = CARTESIAN_POINT ( 'NONE',  ( -78.00000000000001421, 67.72792206135787296, -5.742637315201482906 ) ) ;
#10318 = VERTEX_POINT ( 'NONE', #8107 ) ;
#10319 = CARTESIAN_POINT ( 'NONE',  ( -44.66281104389123868, 63.04473320575852568, -19.42304942373100829 ) ) ;
#10320 = CARTESIAN_POINT ( 'NONE',  ( -75.12500000204838102, 29.18810118750000626, -10.69163855873949309 ) ) ;
#10321 = EDGE_CURVE ( 'NONE', #546, #8432, #10957, .T. ) ;
#10322 = VECTOR ( 'NONE', #2283, 1000.000000000000000 ) ;
#10323 = EDGE_CURVE ( 'NONE', #1033, #1850, #7217, .T. ) ;
#10324 = CYLINDRICAL_SURFACE ( 'NONE', #10359, 24.99999999999999645 ) ;
#10325 = CARTESIAN_POINT ( 'NONE',  ( -45.81092964171354964, 71.80742102382775727, -12.92463648794852205 ) ) ;
#10326 = SURFACE_SIDE_STYLE ('',( #9429 ) ) ;
#10327 = ORIENTED_EDGE ( 'NONE', *, *, #3083, .F. ) ;
#10328 = CARTESIAN_POINT ( 'NONE',  ( -72.03125000204839523, 36.74823131438024859, -18.25176868561973720 ) ) ;
#10329 = CARTESIAN_POINT ( 'NONE',  ( -72.59375000409677625, 80.00000000000001421, -10.35533905932737753 ) ) ;
#10330 = CIRCLE ( 'NONE', #2107, 2.445500000000003116 ) ;
#10331 = CARTESIAN_POINT ( 'NONE',  ( 2.003855453843550460, 35.57695044197526357, -8.044733130177707636 ) ) ;
#10332 = ORIENTED_EDGE ( 'NONE', *, *, #2646, .T. ) ;
#10333 = CARTESIAN_POINT ( 'NONE',  ( -65.14229033403913149, 38.19691209738603277, 12.92632704043474412 ) ) ;
#10334 = CARTESIAN_POINT ( 'NONE',  ( -44.07074648197151845, 61.10275710191199749, -20.11236068975357938 ) ) ;
#10335 = CARTESIAN_POINT ( 'NONE',  ( -78.96875000000001421, 30.00000000000003908, 10.35533905932737753 ) ) ;
#10336 = EDGE_CURVE ( 'NONE', #193, #6797, #2496, .T. ) ;
#10337 = VECTOR ( 'NONE', #9662, 1000.000000000000000 ) ;
#10338 = CARTESIAN_POINT ( 'NONE',  ( 36.99999999999999289, 64.99999999999998579, 0.000000000000000000 ) ) ;
#10339 = CARTESIAN_POINT ( 'NONE',  ( 36.99999999999999289, 55.00000000000000000, 5.249999999999998224 ) ) ;
#10340 = ORIENTED_EDGE ( 'NONE', *, *, #1143, .F. ) ;
#10341 = CARTESIAN_POINT ( 'NONE',  ( -74.93750000000000000, 72.67766952966368876, 17.67766952966368521 ) ) ;
#10342 = CARTESIAN_POINT ( 'NONE',  ( -20.00000000000003197, -63.00000000000000000, 5.000000000000000000 ) ) ;
#10343 = CONICAL_SURFACE ( 'NONE', #2, 3.000000000000000000, 0.9599310885968912466 ) ;
#10344 = CARTESIAN_POINT ( 'NONE',  ( -77.09375000000004263, 44.64466094067264379, -24.99999999999989697 ) ) ;
#10345 = CIRCLE ( 'NONE', #7119, 3.000000000000002665 ) ;
#10346 = AXIS2_PLACEMENT_3D ( 'NONE', #2229, #4875, #11263 ) ;
#10347 = CARTESIAN_POINT ( 'NONE',  ( -76.25000000000000000, 55.00000000000000000, 24.99999999999999645 ) ) ;
#10348 = CARTESIAN_POINT ( 'NONE',  ( -62.78770230684006748, 51.59540953287255860, 13.59211127035758260 ) ) ;
#10349 = ORIENTED_EDGE ( 'NONE', *, *, #3751, .T. ) ;
#10350 = CARTESIAN_POINT ( 'NONE',  ( -7.969360823174009845, 70.58422527244209732, -14.12522777056770629 ) ) ;
#10351 = DIRECTION ( 'NONE',  ( -9.813077866773612233E-16, 1.000000000000000000, 0.000000000000000000 ) ) ;
#10352 = CYLINDRICAL_SURFACE ( 'NONE', #7552, 1.499999999999999556 ) ;
#10353 = CARTESIAN_POINT ( 'NONE',  ( 36.99999999999999289, 55.00000000000000000, 0.000000000000000000 ) ) ;
#10354 = CARTESIAN_POINT ( 'NONE',  ( -14.94198242393282605, 71.73612833094152563, 18.58153189695169161 ) ) ;
#10355 = CARTESIAN_POINT ( 'NONE',  ( -77.28125000204839523, 73.25176868561975141, 18.25176868561974075 ) ) ;
#10356 = EDGE_LOOP ( 'NONE', ( #8472, #7377, #10706, #4050 ) ) ;
#10357 = CARTESIAN_POINT ( 'NONE',  ( -71.34302368722833876, 77.35376350879521112, 12.90594348738575903 ) ) ;
#10358 = CIRCLE ( 'NONE', #4816, 1.500000000000001332 ) ;
#10359 = AXIS2_PLACEMENT_3D ( 'NONE', #3983, #2907, #7527 ) ;
#10360 = FACE_BOUND ( 'NONE', #731, .T. ) ;
#10361 = CARTESIAN_POINT ( 'NONE',  ( 20.68439517297596453, 76.14615934997016211, -13.34036362221765692 ) ) ;
#10362 = CARTESIAN_POINT ( 'NONE',  ( -30.07727491738399905, 41.06011215405257531, 1.372365971865714407 ) ) ;
#10363 = FACE_OUTER_BOUND ( 'NONE', #6286, .T. ) ;
#10364 =( BOUNDED_CURVE ( )  B_SPLINE_CURVE ( 2, ( #6461, #10214, #2975, #147, #5679, #7417, #9320, #9144, #1951 ),
 .UNSPECIFIED., .F., .T. ) 
 B_SPLINE_CURVE_WITH_KNOTS ( ( 3, 2, 2, 2, 3 ),
 ( 0.5833333333333338144, 0.6041666666666670737, 0.6250000000000004441, 0.6458333333333339255, 0.6666666666666671848 ),
 .UNSPECIFIED. ) 
 CURVE ( )  GEOMETRIC_REPRESENTATION_ITEM ( )  RATIONAL_B_SPLINE_CURVE ( ( 0.9999999999999983347, 0.9238795325112884038, 1.000000000000000000, 0.9238795325112867385, 1.000000000000000000, 0.9238795325112867385, 1.000000000000000000, 0.9238795325112847401, 1.000000000000001998 ) ) 
 REPRESENTATION_ITEM ( '' )  );
#10365 = CARTESIAN_POINT ( 'NONE',  ( -80.00000000000000000, 54.99999999999999289, 1.500003371917797201 ) ) ;
#10366 = DIRECTION ( 'NONE',  ( 0.000000000000000000, -0.000000000000000000, 1.000000000000000000 ) ) ;
#10367 = ORIENTED_EDGE ( 'NONE', *, *, #6293, .F. ) ;
#10368 = CARTESIAN_POINT ( 'NONE',  ( -72.68750000000000000, 37.32233047033631124, -17.67766952966368166 ) ) ;
#10369 = DIRECTION ( 'NONE',  ( -1.000000000000000000, 0.000000000000000000, 0.000000000000000000 ) ) ;
#10370 = PLANE ( 'NONE',  #1921 ) ;
#10371 = ORIENTED_EDGE ( 'NONE', *, *, #2334, .F. ) ;
#10372 = ADVANCED_FACE ( 'NONE', ( #6376 ), #1686, .F. ) ;
#10373 = CARTESIAN_POINT ( 'NONE',  ( -12.44324757165961870, 62.02537596287093891, 0.9163237194946400876 ) ) ;
#10374 = DIRECTION ( 'NONE',  ( 0.000000000000000000, 0.000000000000000000, 1.000000000000000000 ) ) ;
#10375 = CARTESIAN_POINT ( 'NONE',  ( 0.000000000000000000, -57.00000000000000000, 5.000000000000000000 ) ) ;
#10376 = ORIENTED_EDGE ( 'NONE', *, *, #3103, .F. ) ;
#10377 = CARTESIAN_POINT ( 'NONE',  ( -79.43750000000004263, 72.67766952966367455, 17.67766952966366745 ) ) ;
#10378 = CARTESIAN_POINT ( 'NONE',  ( -77.18750000204838102, 44.30836144126052289, 25.81189881250000795 ) ) ;
#10379 = ORIENTED_EDGE ( 'NONE', *, *, #6682, .T. ) ;
#10380 = CARTESIAN_POINT ( 'NONE',  ( -54.88146047731135013, 73.03677976846768161, 10.81065700633557825 ) ) ;
#10381 = CARTESIAN_POINT ( 'NONE',  ( -74.28125000204839523, 73.25176868561975141, 18.25176868561974075 ) ) ;
#10382 = ADVANCED_FACE ( 'NONE', ( #10781 ), #10085, .F. ) ;
#10383 = DIRECTION ( 'NONE',  ( 1.000000000000000000, 0.000000000000000000, 0.000000000000000000 ) ) ;
#10384 = CARTESIAN_POINT ( 'NONE',  ( -63.06671435217206323, 41.62111505249539078, 16.30162306856191989 ) ) ;
#10385 = FACE_OUTER_BOUND ( 'NONE', #11795, .T. ) ;
#10386 = ORIENTED_EDGE ( 'NONE', *, *, #2334, .T. ) ;
#10387 = CARTESIAN_POINT ( 'NONE',  ( 34.00000000000000000, 55.00000000000000000, 0.000000000000000000 ) ) ;
#10388 = CARTESIAN_POINT ( 'NONE',  ( -2.287832656137187115, 4.452621892014636096, 3.582384678254184149E-15 ) ) ;
#10389 = CARTESIAN_POINT ( 'NONE',  ( -19.00387657603030078, 69.86840152515847535, 14.86901714484747750 ) ) ;
#10390 = EDGE_LOOP ( 'NONE', ( #854, #858, #7608, #3020, #2252, #3711 ) ) ;
#10391 = CARTESIAN_POINT ( 'NONE',  ( -3.522319526695277148, 52.25407378758720256, -20.97954707081091996 ) ) ;
#10392 = CARTESIAN_POINT ( 'NONE',  ( 7.872895456215955434, 43.79306672811842560, 8.617525609973794687 ) ) ;
#10393 = CARTESIAN_POINT ( 'NONE',  ( -15.00000000000000000, -30.00000000000000000, -10.00000000000000000 ) ) ;
#10394 = DIRECTION ( 'NONE',  ( -1.000000000000000000, -0.000000000000000000, -0.000000000000000000 ) ) ;
#10395 = CARTESIAN_POINT ( 'NONE',  ( -3.000000000000000000, 0.000000000000000000, -1.753742857142857048 ) ) ;
#10396 = ORIENTED_EDGE ( 'NONE', *, *, #5219, .T. ) ;
#10397 = CARTESIAN_POINT ( 'NONE',  ( -75.78125000000001421, 30.00000000000000355, -10.35533905932738108 ) ) ;
#10398 = CARTESIAN_POINT ( 'NONE',  ( -61.71391363462142010, 54.99991449564567603, -0.005034624627165642033 ) ) ;
#10399 = VECTOR ( 'NONE', #8682, 1000.000000000000000 ) ;
#10400 = ADVANCED_FACE ( 'NONE', ( #893 ), #5588, .F. ) ;
#10401 = LINE ( 'NONE', #11296, #10542 ) ;
#10402 = CARTESIAN_POINT ( 'NONE',  ( 22.99999999999999645, 76.00000000000000000, 0.000000000000000000 ) ) ;
#10403 = CARTESIAN_POINT ( 'NONE',  ( -65.40872037032744402, 46.08084772439340071, 10.86636812464517376 ) ) ;
#10404 = ORIENTED_EDGE ( 'NONE', *, *, #11012, .F. ) ;
#10405 = CARTESIAN_POINT ( 'NONE',  ( -25.52231952398968673, 42.10919693116569817, 16.77412918608628090 ) ) ;
#10406 = EDGE_CURVE ( 'NONE', #52, #6251, #11424, .T. ) ;
#10407 = CARTESIAN_POINT ( 'NONE',  ( 0.000000000000000000, 0.000000000000000000, -6.099999999999999645 ) ) ;
#10408 = FACE_BOUND ( 'NONE', #6882, .T. ) ;
#10409 = EDGE_CURVE ( 'NONE', #10526, #1709, #7449, .T. ) ;
#10410 = CARTESIAN_POINT ( 'NONE',  ( -77.93750000204838102, 44.30836144126049447, -25.81189881249999019 ) ) ;
#10411 = CARTESIAN_POINT ( 'NONE',  ( 39.99999999999999289, 55.00000000000000000, 0.000000000000000000 ) ) ;
#10412 = CARTESIAN_POINT ( 'NONE',  ( -72.12500000204839523, 44.30836144126050158, -25.81189881249999374 ) ) ;
#10413 = ORIENTED_EDGE ( 'NONE', *, *, #5587, .T. ) ;
#10414 = CARTESIAN_POINT ( 'NONE',  ( -74.00000000204840944, 44.30836144126053000, 25.81189881250000795 ) ) ;
#10415 = LINE ( 'NONE', #11423, #8459 ) ;
#10416 = CARTESIAN_POINT ( 'NONE',  ( -66.46433446062644634, 41.33748651086542480, 3.672754829735058735 ) ) ;
#10417 = DIRECTION ( 'NONE',  ( -1.000000000000000000, 0.000000000000000000, 0.000000000000000000 ) ) ;
#10418 = CARTESIAN_POINT ( 'NONE',  ( -78.00000000000002842, 46.51471862576140381, 3.371917798797308130E-06 ) ) ;
#10419 = DIRECTION ( 'NONE',  ( -1.000000000000000000, -0.000000000000000000, -0.000000000000000000 ) ) ;
#10420 =( GEOMETRIC_REPRESENTATION_CONTEXT ( 3 ) GLOBAL_UNCERTAINTY_ASSIGNED_CONTEXT ( ( #6768 ) ) GLOBAL_UNIT_ASSIGNED_CONTEXT ( ( #11276, #7995, #7818 ) ) REPRESENTATION_CONTEXT ( 'NONE', 'WORKASPACE' ) );
#10421 = ORIENTED_EDGE ( 'NONE', *, *, #6831, .T. ) ;
#10422 = CARTESIAN_POINT ( 'NONE',  ( -73.06250000000000000, 37.32233047033631124, 17.67766952966369232 ) ) ;
#10423 = CARTESIAN_POINT ( 'NONE',  ( -73.06250000409677625, 37.32233047033631124, -17.67766952966368166 ) ) ;
#10424 = CARTESIAN_POINT ( 'NONE',  ( -75.00000000000000000, 55.00000000000000000, 0.000000000000000000 ) ) ;
#10425 = VERTEX_POINT ( 'NONE', #5772 ) ;
#10426 = CARTESIAN_POINT ( 'NONE',  ( 25.66666666666666430, 61.99999999999997868, 0.000000000000000000 ) ) ;
#10427 = LINE ( 'NONE', #1267, #9594 ) ;
#10428 = DIRECTION ( 'NONE',  ( 0.000000000000000000, 0.000000000000000000, 1.000000000000000000 ) ) ;
#10429 = VERTEX_POINT ( 'NONE', #11192 ) ;
#10430 = CARTESIAN_POINT ( 'NONE',  ( 7.004752486429524083, 66.69611028691875276, -18.63618820634359352 ) ) ;
#10431 = CARTESIAN_POINT ( 'NONE',  ( -79.53125000204838102, 55.00000000000000000, -25.81189881249999729 ) ) ;
#10432 = ORIENTED_EDGE ( 'NONE', *, *, #4332, .F. ) ;
#10433 = CARTESIAN_POINT ( 'NONE',  ( -47.81092963715463640, 71.80394787507084686, -12.92116392654651058 ) ) ;
#10434 = CARTESIAN_POINT ( 'NONE',  ( -74.93750000204839523, 44.30836144126050158, -25.81189881249999374 ) ) ;
#10435 = DIRECTION ( 'NONE',  ( 0.8191520442889974607, 1.003171929053531649E-16, -0.5735764363510379438 ) ) ;
#10436 = CARTESIAN_POINT ( 'NONE',  ( -66.81799029952708224, 34.52069382205590387, 5.503409927558503334 ) ) ;
#10437 = PRESENTATION_STYLE_ASSIGNMENT (( #10263 ) ) ;
#10438 = CARTESIAN_POINT ( 'NONE',  ( 2.500000000000000000, 0.000000000000000000, -5.560532340533429263 ) ) ;
#10439 = VERTEX_POINT ( 'NONE', #5712 ) ;
#10440 = CARTESIAN_POINT ( 'NONE',  ( -30.23830917210572267, 50.00000000000000711, 1.120793995806890209E-14 ) ) ;
#10441 = CARTESIAN_POINT ( 'NONE',  ( -14.31788144970486165, 59.96719419353341607, -0.6577655422762530568 ) ) ;
#10442 = CARTESIAN_POINT ( 'NONE',  ( -32.40407992077046373, 34.08317752212569474, 2.058454929014103651 ) ) ;
#10443 = ORIENTED_EDGE ( 'NONE', *, *, #2922, .T. ) ;
#10444 = ADVANCED_FACE ( 'NONE', ( #6489 ), #4926, .T. ) ;
#10445 = CARTESIAN_POINT ( 'NONE',  ( -10.72515708486913866, 73.59929058593817786, -9.932910085056876781 ) ) ;
#10446 = CARTESIAN_POINT ( 'NONE',  ( -2.206240550821941593, 47.95770083149849228, -12.21699568532449121 ) ) ;
#10447 = LINE ( 'NONE', #10393, #6499 ) ;
#10448 = CARTESIAN_POINT ( 'NONE',  ( 39.99999999999999289, 55.00000000000000000, 24.99999999999999645 ) ) ;
#10449 = CONICAL_SURFACE ( 'NONE', #10262, 3.000000000000000000, 0.9599310885968912466 ) ;
#10450 = CARTESIAN_POINT ( 'NONE',  ( -67.56971494453328830, 50.00000002031717372, -0.0004507456344833478141 ) ) ;
#10451 = ORIENTED_EDGE ( 'NONE', *, *, #5820, .F. ) ;
#10452 = CARTESIAN_POINT ( 'NONE',  ( -78.03124999999998579, 80.00000000000001421, 10.35533905932737397 ) ) ;
#10453 = LINE ( 'NONE', #6713, #8920 ) ;
#10454 = DIRECTION ( 'NONE',  ( -1.000000000000000000, -0.000000000000000000, -0.000000000000000000 ) ) ;
#10455 = AXIS2_PLACEMENT_3D ( 'NONE', #633, #7396, #1537 ) ;
#10456 = DIRECTION ( 'NONE',  ( 0.000000000000000000, 1.000000000000000000, 0.000000000000000000 ) ) ;
#10457 = CARTESIAN_POINT ( 'NONE',  ( -10.62461255960855233, 60.19719913025998181, -4.710188242643384093 ) ) ;
#10458 = AXIS2_PLACEMENT_3D ( 'NONE', #1734, #3654, #11788 ) ;
#10459 = VERTEX_POINT ( 'NONE', #10303 ) ;
#10460 = CARTESIAN_POINT ( 'NONE',  ( -13.14429486149114013, 76.02373996650987920, 2.745652855075435994 ) ) ;
#10461 = DIRECTION ( 'NONE',  ( 0.000000000000000000, 0.000000000000000000, 1.000000000000000000 ) ) ;
#10462 = ADVANCED_FACE ( 'NONE', ( #1919 ), #5646, .F. ) ;
#10463 = CARTESIAN_POINT ( 'NONE',  ( -78.00000000000001421, 71.97056274847716395, -1.499996628082204797 ) ) ;
#10464 = CARTESIAN_POINT ( 'NONE',  ( -78.87500000204839523, 80.81189881250000440, 10.69163855873948243 ) ) ;
#10465 = CARTESIAN_POINT ( 'NONE',  ( -76.06250000000005684, 37.32233047033638940, 17.67766952966361771 ) ) ;
#10466 = CARTESIAN_POINT ( 'NONE',  ( -72.12500000204840944, 29.18810118750000626, -10.69163855873949309 ) ) ;
#10467 = ORIENTED_EDGE ( 'NONE', *, *, #1168, .F. ) ;
#10468 = CARTESIAN_POINT ( 'NONE',  ( -78.12500000409677625, 55.00000000000000000, 24.99999999999999645 ) ) ;
#10469 = FACE_OUTER_BOUND ( 'NONE', #6567, .T. ) ;
#10470 = CARTESIAN_POINT ( 'NONE',  ( -78.00000000000001421, 59.24264068711928388, -11.22791868944003824 ) ) ;
#10471 = AXIS2_PLACEMENT_3D ( 'NONE', #4018, #5642, #1251 ) ;
#10472 = CARTESIAN_POINT ( 'NONE',  ( 12.52240408941406535, 44.41801188983610871, 18.37272825892985040 ) ) ;
#10473 = ADVANCED_FACE ( 'NONE', ( #1077 ), #4744, .T. ) ;
#10474 = CARTESIAN_POINT ( 'NONE',  ( -78.00000000000000000, 54.99999999999999289, 0.000000000000000000 ) ) ;
#10475 = DIRECTION ( 'NONE',  ( 0.000000000000000000, 0.000000000000000000, -1.000000000000000000 ) ) ;
#10476 = CARTESIAN_POINT ( 'NONE',  ( -78.00000000000001421, 67.72792206135787296, -5.742637315201482906 ) ) ;
#10477 = VECTOR ( 'NONE', #1856, 1000.000000000000000 ) ;
#10478 = VERTEX_POINT ( 'NONE', #3963 ) ;
#10479 = FACE_OUTER_BOUND ( 'NONE', #2353, .T. ) ;
#10480 = CARTESIAN_POINT ( 'NONE',  ( -72.40625000000000000, 65.35533905932737753, -24.99999999999999645 ) ) ;
#10481 = CARTESIAN_POINT ( 'NONE',  ( -71.18750000409677625, 72.67766952966368876, -17.67766952966368876 ) ) ;
#10482 = EDGE_CURVE ( 'NONE', #8176, #9472, #8581, .T. ) ;
#10483 = DIRECTION ( 'NONE',  ( -0.000000000000000000, -0.000000000000000000, -1.000000000000000000 ) ) ;
#10484 = ORIENTED_EDGE ( 'NONE', *, *, #3354, .T. ) ;
#10485 = CARTESIAN_POINT ( 'NONE',  ( -53.08379927897976813, 60.41024208566564369, 4.439607033037889394 ) ) ;
#10486 = DIRECTION ( 'NONE',  ( 0.000000000000000000, 1.000000000000000000, 0.000000000000000000 ) ) ;
#10487 = FILL_AREA_STYLE ('',( #7692 ) ) ;
#10488 = EDGE_LOOP ( 'NONE', ( #2037, #8966, #4440, #7061, #10592, #3916 ) ) ;
#10489 = CARTESIAN_POINT ( 'NONE',  ( 16.75908867079492737, 72.98228652723742016, 12.73316312262223171 ) ) ;
#10490 = CARTESIAN_POINT ( 'NONE',  ( -77.46875000204839523, 73.25176868561975141, 18.25176868561974075 ) ) ;
#10491 = AXIS2_PLACEMENT_3D ( 'NONE', #632, #4294, #7066 ) ;
#10492 = ORIENTED_EDGE ( 'NONE', *, *, #4994, .F. ) ;
#10493 = LINE ( 'NONE', #7753, #9173 ) ;
#10494 = FACE_OUTER_BOUND ( 'NONE', #4933, .T. ) ;
#10495 = CARTESIAN_POINT ( 'NONE',  ( -79.53125000000001421, 79.99999999999998579, 10.35533905932735799 ) ) ;
#10496 = CIRCLE ( 'NONE', #7081, 20.00000000000000355 ) ;
#10497 =( NAMED_UNIT ( * ) PLANE_ANGLE_UNIT ( ) SI_UNIT ( $, .RADIAN. ) );
#10498 = VECTOR ( 'NONE', #2369, 1000.000000000000000 ) ;
#10499 = DIRECTION ( 'NONE',  ( 1.000000000000000000, 0.000000000000000000, 0.000000000000000000 ) ) ;
#10500 = EDGE_LOOP ( 'NONE', ( #7944, #6234, #4901, #7535 ) ) ;
#10501 = DIRECTION ( 'NONE',  ( -1.000000000000000000, -0.000000000000000000, -0.000000000000000000 ) ) ;
#10502 = CARTESIAN_POINT ( 'NONE',  ( -43.21475900837984341, 58.08538667521604282, -20.80084980650556759 ) ) ;
#10503 = ORIENTED_EDGE ( 'NONE', *, *, #5219, .F. ) ;
#10504 = CARTESIAN_POINT ( 'NONE',  ( 4.118574298861553906, 34.19883370460495087, -3.085387377675621767 ) ) ;
#10505 = VECTOR ( 'NONE', #5498, 999.9999999999998863 ) ;
#10506 = CARTESIAN_POINT ( 'NONE',  ( -44.12197311277270728, 58.40423241926509235, -13.59316381755316350 ) ) ;
#10507 = CARTESIAN_POINT ( 'NONE',  ( -15.00000000000000355, 5.000000000000000000, 30.00000000000000711 ) ) ;
#10508 =( NAMED_UNIT ( * ) PLANE_ANGLE_UNIT ( ) SI_UNIT ( $, .RADIAN. ) );
#10509 = AXIS2_PLACEMENT_3D ( 'NONE', #5326, #8252, #4541 ) ;
#10510 = DIRECTION ( 'NONE',  ( 0.000000000000000000, 1.000000000000000000, 0.000000000000000000 ) ) ;
#10511 = ORIENTED_EDGE ( 'NONE', *, *, #9786, .F. ) ;
#10512 = CARTESIAN_POINT ( 'NONE',  ( -78.87500000204838102, 65.69163855873949842, 25.81189881250000440 ) ) ;
#10513 = CARTESIAN_POINT ( 'NONE',  ( -66.09273081889568857, 55.00395080879571452, -0.007536095274406174466 ) ) ;
#10514 = EDGE_CURVE ( 'NONE', #4655, #2578, #7511, .T. ) ;
#10515 = CARTESIAN_POINT ( 'NONE',  ( -78.00000000000002842, 46.51471862576140381, 9.985284746156354529 ) ) ;
#10516 = CARTESIAN_POINT ( 'NONE',  ( -33.08380120443626993, 48.03207042869781418, 0.6864286361564611028 ) ) ;
#10517 = ORIENTED_EDGE ( 'NONE', *, *, #5055, .T. ) ;
#10518 = CARTESIAN_POINT ( 'NONE',  ( -20.50647613538409075, 59.12524989819403487, 20.69783765389080799 ) ) ;
#10519 = DIRECTION ( 'NONE',  ( -0.8191520442889885789, 1.003171929053520802E-16, 0.5735764363510507113 ) ) ;
#10520 = DIRECTION ( 'NONE',  ( -1.000000000000000000, -0.000000000000000000, -0.000000000000000000 ) ) ;
#10521 = ADVANCED_FACE ( 'NONE', ( #7384 ), #6674, .F. ) ;
#10522 = CARTESIAN_POINT ( 'NONE',  ( -74.46875000204839523, 80.81189881250000440, -1.580522963032174394E-15 ) ) ;
#10523 = CARTESIAN_POINT ( 'NONE',  ( -16.16012453410070293, 72.62154289115962058, 17.74408479697386554 ) ) ;
#10524 = CARTESIAN_POINT ( 'NONE',  ( -75.96875000204839523, 80.81189881250000440, -1.580522963032174394E-15 ) ) ;
#10525 = CIRCLE ( 'NONE', #6917, 30.57961884250791940 ) ;
#10526 = VERTEX_POINT ( 'NONE', #178 ) ;
#10527 = CARTESIAN_POINT ( 'NONE',  ( -72.78125000409679046, 65.35533905932737753, -24.99999999999999645 ) ) ;
#10528 = DIRECTION ( 'NONE',  ( 0.000000000000000000, 0.000000000000000000, 1.000000000000000000 ) ) ;
#10529 = VERTEX_POINT ( 'NONE', #8462 ) ;
#10530 = PRODUCT ( 'hex nut gradec_iso_ISO - 4034 - M6 - S', 'hex nut gradec_iso_ISO - 4034 - M6 - S', '', ( #10125 ) ) ;
#10531 = CARTESIAN_POINT ( 'NONE',  ( 7.506399388638331338, 34.30832474160909129, 4.109400874309620200 ) ) ;
#10532 = AXIS2_PLACEMENT_3D ( 'NONE', #657, #4265, #4205 ) ;
#10533 = AXIS2_PLACEMENT_3D ( 'NONE', #607, #1395, #3361 ) ;
#10534 = CARTESIAN_POINT ( 'NONE',  ( -78.00000000000001421, 67.72792206135787296, 11.22792543327562775 ) ) ;
#10535 = CARTESIAN_POINT ( 'NONE',  ( 14.99999999999999645, 0.000000000000000000, 10.00000000000000178 ) ) ;
#10536 = DIRECTION ( 'NONE',  ( -0.000000000000000000, -0.000000000000000000, 1.000000000000000000 ) ) ;
#10537 = EDGE_CURVE ( 'NONE', #1675, #2759, #11075, .T. ) ;
#10538 = ORIENTED_EDGE ( 'NONE', *, *, #10007, .T. ) ;
#10539 = CARTESIAN_POINT ( 'NONE',  ( -79.43750000204838102, 55.00000000000000000, -24.99999999999999645 ) ) ;
#10540 = ADVANCED_FACE ( 'NONE', ( #10186 ), #7568, .F. ) ;
#10541 = EDGE_CURVE ( 'NONE', #8040, #3221, #11134, .T. ) ;
#10542 = VECTOR ( 'NONE', #11114, 1000.000000000000000 ) ;
#10543 = CARTESIAN_POINT ( 'NONE',  ( -75.03125000000000000, 80.00000000000001421, 10.35533905932737397 ) ) ;
#10544 = CARTESIAN_POINT ( 'NONE',  ( -15.00000000000000000, -30.00000000000000000, -10.00000000000000000 ) ) ;
#10545 = PLANE ( 'NONE',  #6736 ) ;
#10546 = ORIENTED_EDGE ( 'NONE', *, *, #6989, .T. ) ;
#10547 = CARTESIAN_POINT ( 'NONE',  ( -41.41713581769108998, 57.03123113432517499, -6.697302567478903512 ) ) ;
#10548 = EDGE_CURVE ( 'NONE', #5996, #2213, #10240, .T. ) ;
#10549 = EDGE_CURVE ( 'NONE', #7713, #6771, #3023, .T. ) ;
#10550 = DIRECTION ( 'NONE',  ( 0.000000000000000000, 0.000000000000000000, 1.000000000000000000 ) ) ;
#10551 = VECTOR ( 'NONE', #11388, 1000.000000000000000 ) ;
#10552 = EDGE_CURVE ( 'NONE', #8651, #3207, #8517, .T. ) ;
#10553 = ORIENTED_EDGE ( 'NONE', *, *, #6263, .T. ) ;
#10554 = CARTESIAN_POINT ( 'NONE',  ( 21.49621555244012328, 76.81665687444413493, 2.927878090024194968 ) ) ;
#10555 = CARTESIAN_POINT ( 'NONE',  ( -2.287832656137187115, 4.452621892014636984, -6.100000000000003197 ) ) ;
#10556 = EDGE_LOOP ( 'NONE', ( #10808, #9687 ) ) ;
#10557 = CARTESIAN_POINT ( 'NONE',  ( -73.43750000204839523, 44.30836144126050158, -25.81189881249999374 ) ) ;
#10558 = DIRECTION ( 'NONE',  ( -1.000000000000000000, -0.000000000000000000, -0.000000000000000000 ) ) ;
#10559 = DIRECTION ( 'NONE',  ( 0.000000000000000000, 1.000000000000000000, 0.000000000000000000 ) ) ;
#10560 = CARTESIAN_POINT ( 'NONE',  ( 7.618938171403620174, 55.00878100866180631, 0.0002433764497684456950 ) ) ;
#10561 = CARTESIAN_POINT ( 'NONE',  ( -75.00000000000001421, 34.09894944383669468, 14.06340364766198725 ) ) ;
#10562 = VERTEX_POINT ( 'NONE', #3720 ) ;
#10563 = LINE ( 'NONE', #3263, #889 ) ;
#10564 = CARTESIAN_POINT ( 'NONE',  ( -50.14429338685609849, 75.46958046783008456, -5.506903914760000518 ) ) ;
#10565 = VERTEX_POINT ( 'NONE', #2277 ) ;
#10566 = CARTESIAN_POINT ( 'NONE',  ( 0.9415095817738947659, 38.70554731314401664, -13.38234376684299143 ) ) ;
#10567 = CARTESIAN_POINT ( 'NONE',  ( -39.53949924438659025, 47.95754239612929837, -12.21692829552484660 ) ) ;
#10568 = DIRECTION ( 'NONE',  ( -1.000000000000000000, -0.000000000000000000, -0.000000000000000000 ) ) ;
#10569 = CARTESIAN_POINT ( 'NONE',  ( -24.81855061910753690, 54.66933223131182729, 4.999996196634724832 ) ) ;
#10570 = ORIENTED_EDGE ( 'NONE', *, *, #1332, .F. ) ;
#10571 = CARTESIAN_POINT ( 'NONE',  ( -71.91717626682689968, 72.42551787026226862, 19.81812247078860523 ) ) ;
#10572 = CARTESIAN_POINT ( 'NONE',  ( -80.00000000000002842, 42.27207793864211283, 5.742644059037075088 ) ) ;
#10573 = DIRECTION ( 'NONE',  ( -1.000000000000000000, -0.000000000000000000, -0.000000000000000000 ) ) ;
#10574 = CARTESIAN_POINT ( 'NONE',  ( -78.00000000000001421, 67.72792206135787296, -14.22791868944004356 ) ) ;
#10575 = CARTESIAN_POINT ( 'NONE',  ( -54.66652844283319723, 61.47673604987254237, 2.683042620825347058 ) ) ;
#10576 = ORIENTED_EDGE ( 'NONE', *, *, #3567, .T. ) ;
#10577 = CARTESIAN_POINT ( 'NONE',  ( -30.11869220662914159, 34.20731585996448132, 3.085050890631813036 ) ) ;
#10578 = CARTESIAN_POINT ( 'NONE',  ( 4.636023424558444184, 34.00634798409771520, 1.031279783234476222 ) ) ;
#10579 = DIRECTION ( 'NONE',  ( -0.000000000000000000, -1.000000000000000000, -0.000000000000000000 ) ) ;
#10580 = CARTESIAN_POINT ( 'NONE',  ( -76.71875000204839523, 29.18810118750000271, 4.741568889096522788E-15 ) ) ;
#10581 = EDGE_CURVE ( 'NONE', #1342, #3861, #9590, .T. ) ;
#10582 = CARTESIAN_POINT ( 'NONE',  ( 36.99999999999999289, 55.00000000000000000, 0.000000000000000000 ) ) ;
#10583 = CARTESIAN_POINT ( 'NONE',  ( -74.46875000204839523, 80.81189881250000440, -1.580522963032174394E-15 ) ) ;
#10584 = ORIENTED_EDGE ( 'NONE', *, *, #1838, .F. ) ;
#10585 = CARTESIAN_POINT ( 'NONE',  ( -71.00000000409677625, 80.00000000000000000, -1.530808498934191324E-15 ) ) ;
#10586 = DIRECTION ( 'NONE',  ( -0.000000000000000000, -0.000000000000000000, -1.000000000000000000 ) ) ;
#10587 = CARTESIAN_POINT ( 'NONE',  ( -71.93750000409677625, 37.32233047033631124, 17.67766952966369232 ) ) ;
#10588 = CARTESIAN_POINT ( 'NONE',  ( 2.274842917244503937, 38.70728229458904934, -13.38060881307704975 ) ) ;
#10589 = CARTESIAN_POINT ( 'NONE',  ( -77.93750000204838102, 65.69163855873948421, -25.81189881250000084 ) ) ;
#10590 = LINE ( 'NONE', #2391, #6270 ) ;
#10591 = DIRECTION ( 'NONE',  ( 1.000000000000000000, 0.000000000000000000, 0.000000000000000000 ) ) ;
#10592 = ORIENTED_EDGE ( 'NONE', *, *, #5968, .F. ) ;
#10593 = CARTESIAN_POINT ( 'NONE',  ( 53.00000000000000000, 105.0000000000000142, -6.000000000000000000 ) ) ;
#10594 = CARTESIAN_POINT ( 'NONE',  ( -73.15625000000000000, 44.64466094067262958, 25.00000000000001066 ) ) ;
#10595 = DIRECTION ( 'NONE',  ( -1.000000000000000000, -0.000000000000000000, -0.000000000000000000 ) ) ;
#10596 = ORIENTED_EDGE ( 'NONE', *, *, #10695, .T. ) ;
#10597 = DIRECTION ( 'NONE',  ( -1.000000000000000000, 0.000000000000000000, 0.000000000000000000 ) ) ;
#10598 = PRODUCT_DEFINITION_CONTEXT ( 'detailed design', #5793, 'design' ) ;
#10599 = VERTEX_POINT ( 'NONE', #9646 ) ;
#10600 = CARTESIAN_POINT ( 'NONE',  ( -52.20817410683172710, 61.01528383336308536, 3.605005717731896819 ) ) ;
#10601 = CARTESIAN_POINT ( 'NONE',  ( -77.28125000000004263, 30.00000000000009948, -10.35533905932734378 ) ) ;
#10602 = CARTESIAN_POINT ( 'NONE',  ( 9.487511670936607189, 67.96374653773119690, 17.79157655645022373 ) ) ;
#10603 = CARTESIAN_POINT ( 'NONE',  ( -78.00000000000001421, 63.48528137423857487, -6.985278002320760571 ) ) ;
#10604 = ORIENTED_EDGE ( 'NONE', *, *, #7210, .F. ) ;
#10605 = CARTESIAN_POINT ( 'NONE',  ( -77.28125000204839523, 73.25176868561975141, 18.25176868561974075 ) ) ;
#10606 = EDGE_CURVE ( 'NONE', #2912, #9864, #7809, .T. ) ;
#10607 = LINE ( 'NONE', #5179, #2694 ) ;
#10608 = DIRECTION ( 'NONE',  ( 6.033820786006286457E-17, -1.000000000000000000, 0.000000000000000000 ) ) ;
#10609 = CARTESIAN_POINT ( 'NONE',  ( 6.756927758781439586, 54.99032605594245382, -0.0009204374784672792213 ) ) ;
#10610 =( NAMED_UNIT ( * ) PLANE_ANGLE_UNIT ( ) SI_UNIT ( $, .RADIAN. ) );
#10611 = DIRECTION ( 'NONE',  ( 0.000000000000000000, 1.000000000000000000, 0.000000000000000000 ) ) ;
#10612 = EDGE_LOOP ( 'NONE', ( #4275, #11495, #8646 ) ) ;
#10613 = CARTESIAN_POINT ( 'NONE',  ( -75.00000000000001421, 42.56479188213557308, 21.68791366326873060 ) ) ;
#10614 = EDGE_CURVE ( 'NONE', #2344, #3830, #7943, .T. ) ;
#10615 = CARTESIAN_POINT ( 'NONE',  ( -7.929357056070021947, 64.91238717040420170, -18.54984206437098493 ) ) ;
#10616 = ORIENTED_EDGE ( 'NONE', *, *, #9968, .T. ) ;
#10617 = CARTESIAN_POINT ( 'NONE',  ( -24.52239577716529340, 49.50814072396850918, 20.43329749385727112 ) ) ;
#10618 = CARTESIAN_POINT ( 'NONE',  ( -16.20616591473740797, 68.61844237587234829, 3.658903313587498651 ) ) ;
#10619 = CARTESIAN_POINT ( 'NONE',  ( -77.18750000204838102, 44.30836144126053000, 25.81189881250000795 ) ) ;
#10620 = AXIS2_PLACEMENT_3D ( 'NONE', #8799, #578, #520 ) ;
#10621 = ORIENTED_EDGE ( 'NONE', *, *, #2947, .F. ) ;
#10622 = CARTESIAN_POINT ( 'NONE',  ( -79.53125000204838102, 55.00000000000000000, -25.81189881249999729 ) ) ;
#10623 = DIRECTION ( 'NONE',  ( -1.000000000000000000, -0.000000000000000000, -0.000000000000000000 ) ) ;
#10624 = AXIS2_PLACEMENT_3D ( 'NONE', #2230, #9542, #4272 ) ;
#10625 = DIRECTION ( 'NONE',  ( 0.000000000000000000, 0.000000000000000000, 1.000000000000000000 ) ) ;
#10626 = CARTESIAN_POINT ( 'NONE',  ( 20.31540248889015032, 58.05033696222945139, 3.975385948103875577 ) ) ;
#10627 = CARTESIAN_POINT ( 'NONE',  ( -12.08425351220556898, 61.19227081298861037, -3.308756493662277975 ) ) ;
#10628 = ORIENTED_EDGE ( 'NONE', *, *, #8531, .F. ) ;
#10629 = CARTESIAN_POINT ( 'NONE',  ( 3.929252901860227354, 34.88880312433069264, -6.102315970099479792 ) ) ;
#10630 = VECTOR ( 'NONE', #3363, 1000.000000000000000 ) ;
#10631 = CARTESIAN_POINT ( 'NONE',  ( 0.000000000000000000, 5.000000000000000000, 0.000000000000000000 ) ) ;
#10632 = DIRECTION ( 'NONE',  ( -1.000000000000000000, 0.000000000000000000, 0.000000000000000000 ) ) ;
#10633 = ADVANCED_FACE ( 'NONE', ( #11317 ), #5888, .T. ) ;
#10634 = DIRECTION ( 'NONE',  ( -0.000000000000000000, -0.000000000000000000, 1.000000000000000000 ) ) ;
#10635 = CARTESIAN_POINT ( 'NONE',  ( -76.43750000204839523, 44.30836144126050158, -25.81189881249999374 ) ) ;
#10636 = EDGE_LOOP ( 'NONE', ( #626, #3039 ) ) ;
#10637 = CARTESIAN_POINT ( 'NONE',  ( 14.99999999999999645, 0.000000000000000000, 30.00000000000000711 ) ) ;
#10638 = DIRECTION ( 'NONE',  ( -1.000000000000000000, -0.000000000000000000, -0.000000000000000000 ) ) ;
#10639 = CARTESIAN_POINT ( 'NONE',  ( -71.37500000409677625, 55.00000000000000000, -24.99999999999999645 ) ) ;
#10640 = CARTESIAN_POINT ( 'NONE',  ( 8.058385817489730485, 34.79396711235183659, 6.140502173211014103 ) ) ;
#10641 = CONICAL_SURFACE ( 'NONE', #6651, 3.000000000000000888, 0.9599310885968804774 ) ;
#10642 = VERTEX_POINT ( 'NONE', #2220 ) ;
#10643 = CARTESIAN_POINT ( 'NONE',  ( -76.25000000204838102, 80.81189881250000440, -10.69163855873948954 ) ) ;
#10644 = VECTOR ( 'NONE', #5760, 1000.000000000000000 ) ;
#10645 = CARTESIAN_POINT ( 'NONE',  ( 52.99999999999999289, 101.0000000000000000, -9.797174393178809880E-16 ) ) ;
#10646 = B_SPLINE_CURVE_WITH_KNOTS ( 'NONE', 3,
 ( #2452, #8866, #4307, #3406, #10704, #2517, #6181, #5330, #999, #2689, #3701, #3821, #5564, #6592, #7365, #10990, #10940, #1779, #4600, #92, #10878, #11834, #4658, #873, #1896, #7254, #5687, #935, #8311, #5504, #1958, #4546, #1057, #5627, #10222, #4781 ),
 .UNSPECIFIED., .F., .F.,
 ( 4, 2, 2, 2, 2, 2, 2, 2, 2, 2, 2, 2, 2, 2, 2, 2, 2, 4 ),
 ( 0.000000000000000000, 0.001517583048112853628, 0.003035166096225707256, 0.004552749144338561101, 0.006070332192451414512, 0.007587915240564267055, 0.008346706764620690291, 0.009105498288677110058, 0.01214066438490281168, 0.01365824743301567550, 0.01517583048112853931, 0.01593462200518497990, 0.01669341352924142222, 0.01821099657735429297, 0.01972857962546716026, 0.02124616267358003102, 0.02276374572169290525, 0.02428132876980577601 ),
 .UNSPECIFIED. ) ;
#10647 = CARTESIAN_POINT ( 'NONE',  ( 34.00000000000000000, 55.00000000000000000, 0.000000000000000000 ) ) ;
#10648 = CARTESIAN_POINT ( 'NONE',  ( -32.40407992077046373, 34.08317752212569474, 2.058454929014103651 ) ) ;
#10649 = DIRECTION ( 'NONE',  ( 0.000000000000000000, 0.000000000000000000, 1.000000000000000000 ) ) ;
#10650 = AXIS2_PLACEMENT_3D ( 'NONE', #9571, #2144, #1368 ) ;
#10651 = CARTESIAN_POINT ( 'NONE',  ( -77.09375000204839523, 36.74823131438026280, 18.25176868561974786 ) ) ;
#10652 = CARTESIAN_POINT ( 'NONE',  ( -71.09399662003431786, 50.00000004634800632, -0.0006807936302138478625 ) ) ;
#10653 = AXIS2_PLACEMENT_3D ( 'NONE', #4349, #2242, #3323 ) ;
#10654 = VERTEX_POINT ( 'NONE', #10476 ) ;
#10655 = EDGE_CURVE ( 'NONE', #10795, #1798, #3789, .T. ) ;
#10656 = DIRECTION ( 'NONE',  ( -1.000000000000000000, -0.000000000000000000, -0.000000000000000000 ) ) ;
#10657 = ORIENTED_EDGE ( 'NONE', *, *, #8583, .F. ) ;
#10658 = CARTESIAN_POINT ( 'NONE',  ( -29.75046914791206731, 48.03518065199703813, 0.6863338727569227027 ) ) ;
#10659 = APPLICATION_CONTEXT ( 'automotive_design' ) ;
#10660 = CARTESIAN_POINT ( 'NONE',  ( -78.21875000409677625, 65.35533905932734910, 25.00000000000002132 ) ) ;
#10661 = DIRECTION ( 'NONE',  ( -1.000000000000000000, -0.000000000000000000, -0.000000000000000000 ) ) ;
#10662 = PRESENTATION_STYLE_ASSIGNMENT (( #545 ) ) ;
#10663 = CIRCLE ( 'NONE', #9532, 2.500000000000000000 ) ;
#10664 = DIRECTION ( 'NONE',  ( 0.000000000000000000, 0.000000000000000000, 1.000000000000000000 ) ) ;
#10665 = CARTESIAN_POINT ( 'NONE',  ( -74.75000000204838102, 80.81189881250000440, -10.69163855873948954 ) ) ;
#10666 = ORIENTED_EDGE ( 'NONE', *, *, #3274, .T. ) ;
#10667 = CARTESIAN_POINT ( 'NONE',  ( -79.15625000204839523, 73.25176868561975141, -18.25176868561974430 ) ) ;
#10668 = EDGE_CURVE ( 'NONE', #9472, #8176, #338, .T. ) ;
#10669 = CARTESIAN_POINT ( 'NONE',  ( -5.000000000000000000, 1.947085426416875764, -0.1996207071196899330 ) ) ;
#10670 = DIRECTION ( 'NONE',  ( 1.000000000000000000, 6.033820786006286457E-17, 0.000000000000000000 ) ) ;
#10671 = CARTESIAN_POINT ( 'NONE',  ( -3.170201962785300420, 54.99752259272338506, 0.005286603947392433563 ) ) ;
#10672 = CARTESIAN_POINT ( 'NONE',  ( -74.99999999999995737, 39.06450503476944647, 19.38126819931413181 ) ) ;
#10673 = ORIENTED_EDGE ( 'NONE', *, *, #2946, .F. ) ;
#10674 = CARTESIAN_POINT ( 'NONE',  ( -27.12855804074951394, 50.66807883178916683, 2.502284342222150570 ) ) ;
#10675 = VECTOR ( 'NONE', #9028, 1000.000000000000000 ) ;
#10676 = DIRECTION ( 'NONE',  ( -1.000000000000000000, -0.000000000000000000, 0.000000000000000000 ) ) ;
#10677 = EDGE_LOOP ( 'NONE', ( #9105, #9615, #5509, #7968 ) ) ;
#10678 = CARTESIAN_POINT ( 'NONE',  ( -40.49360049774279702, 50.89060478259270326, -20.69231637581390260 ) ) ;
#10679 = CARTESIAN_POINT ( 'NONE',  ( -40.92871871552156193, 50.90608857496490458, -13.47236005574864492 ) ) ;
#10680 = CARTESIAN_POINT ( 'NONE',  ( -77.00000000204838102, 29.18810118750000981, 10.69163855873950020 ) ) ;
#10681 = EDGE_CURVE ( 'NONE', #3280, #9431, #476, .T. ) ;
#10682 = EDGE_CURVE ( 'NONE', #8673, #3954, #6125, .T. ) ;
#10683 = ADVANCED_FACE ( 'NONE', ( #7682 ), #6792, .T. ) ;
#10684 = VECTOR ( 'NONE', #3669, 1000.000000000000000 ) ;
#10685 = VERTEX_POINT ( 'NONE', #9531 ) ;
#10686 = CARTESIAN_POINT ( 'NONE',  ( -78.78125000204838102, 55.00000000000000000, 25.81189881249999729 ) ) ;
#10687 = FACE_OUTER_BOUND ( 'NONE', #8298, .T. ) ;
#10688 = EDGE_CURVE ( 'NONE', #4223, #3357, #3218, .T. ) ;
#10689 = EDGE_CURVE ( 'NONE', #1507, #10278, #4946, .T. ) ;
#10690 = CARTESIAN_POINT ( 'NONE',  ( -83.00000000000000000, 55.00000000000000000, -20.00000000000000355 ) ) ;
#10691 = CARTESIAN_POINT ( 'NONE',  ( 21.47836779243698402, 58.76591268667433354, 3.305356925373596155 ) ) ;
#10692 = CARTESIAN_POINT ( 'NONE',  ( -36.77654997417609906, 48.86760992094172451, -3.531900520213358430 ) ) ;
#10693 = AXIS2_PLACEMENT_3D ( 'NONE', #3269, #11226, #4108 ) ;
#10694 = ORIENTED_EDGE ( 'NONE', *, *, #3520, .T. ) ;
#10695 = EDGE_CURVE ( 'NONE', #5411, #5255, #8765, .T. ) ;
#10696 = CARTESIAN_POINT ( 'NONE',  ( -60.73530621856283318, 48.89645762657089278, 20.10868697360108115 ) ) ;
#10697 = FACE_OUTER_BOUND ( 'NONE', #3999, .T. ) ;
#10698 = DIRECTION ( 'NONE',  ( -1.000000000000000000, 0.000000000000000000, 0.000000000000000000 ) ) ;
#10699 = CYLINDRICAL_SURFACE ( 'NONE', #924, 25.00000000000000355 ) ;
#10700 = CARTESIAN_POINT ( 'NONE',  ( -71.46875000204838102, 80.81189881250000440, -1.580522963032174394E-15 ) ) ;
#10701 = EDGE_LOOP ( 'NONE', ( #2437, #9245, #7316, #4214 ) ) ;
#10702 = CARTESIAN_POINT ( 'NONE',  ( -71.84375000409677625, 30.00000000000001421, 10.35533905932739174 ) ) ;
#10703 = CARTESIAN_POINT ( 'NONE',  ( 53.00000000000000000, 51.46446609406726935, 3.535533905932731091 ) ) ;
#10704 = CARTESIAN_POINT ( 'NONE',  ( -65.62689358872800938, 50.25421578100692699, 1.608180852589480070 ) ) ;
#10705 = CARTESIAN_POINT ( 'NONE',  ( 4.003855478097921861, 35.57747403031575573, -8.044509115018048107 ) ) ;
#10706 = ORIENTED_EDGE ( 'NONE', *, *, #7927, .T. ) ;
#10707 = FACE_OUTER_BOUND ( 'NONE', #4293, .T. ) ;
#10708 = CARTESIAN_POINT ( 'NONE',  ( -54.37477180893560558, 59.74454033230625782, 1.611245227688210324 ) ) ;
#10709 = DIRECTION ( 'NONE',  ( 0.000000000000000000, 1.000000000000000000, 0.000000000000000000 ) ) ;
#10710 = AXIS2_PLACEMENT_3D ( 'NONE', #8175, #10676, #9845 ) ;
#10711 = CARTESIAN_POINT ( 'NONE',  ( -56.32961277634869646, 69.86611656190129338, 14.86520567151240080 ) ) ;
#10712 = CARTESIAN_POINT ( 'NONE',  ( 3.346878500200757500, 3.841181488860377247, -6.048595712916176481 ) ) ;
#10713 = CARTESIAN_POINT ( 'NONE',  ( -76.62500000204839523, 44.30836144126050158, -25.81189881249999374 ) ) ;
#10714 = CYLINDRICAL_SURFACE ( 'NONE', #9753, 1.499999999999999556 ) ;
#10715 = EDGE_LOOP ( 'NONE', ( #5889, #5624, #6405, #9624 ) ) ;
#10716 = CARTESIAN_POINT ( 'NONE',  ( -78.00000000000001421, 71.97056274847716395, 3.371917795327861178E-06 ) ) ;
#10717 = AXIS2_PLACEMENT_3D ( 'NONE', #3785, #9288, #4510 ) ;
#10718 = ORIENTED_EDGE ( 'NONE', *, *, #1485, .T. ) ;
#10719 = CARTESIAN_POINT ( 'NONE',  ( -41.12525411544546472, 56.70070297179961472, -6.793461455911497637 ) ) ;
#10720 = AXIS2_PLACEMENT_3D ( 'NONE', #5291, #7434, #3366 ) ;
#10721 = FACE_OUTER_BOUND ( 'NONE', #6843, .T. ) ;
#10722 = DIRECTION ( 'NONE',  ( -1.000000000000000000, -0.000000000000000000, -0.000000000000000000 ) ) ;
#10723 = CARTESIAN_POINT ( 'NONE',  ( 2.500000000000003109, -4.330127018922193649, -6.099999999999999645 ) ) ;
#10724 = AXIS2_PLACEMENT_3D ( 'NONE', #4385, #6017, #6973 ) ;
#10725 = AXIS2_PLACEMENT_3D ( 'NONE', #10474, #11427, #2340 ) ;
#10726 = DIRECTION ( 'NONE',  ( 0.000000000000000000, 1.000000000000000000, 0.000000000000000000 ) ) ;
#10727 = ORIENTED_EDGE ( 'NONE', *, *, #8402, .F. ) ;
#10728 = CARTESIAN_POINT ( 'NONE',  ( -78.00000000000001421, 67.72792206135787296, 14.22792543327562775 ) ) ;
#10729 = CARTESIAN_POINT ( 'NONE',  ( -78.31250000204839523, 29.18810118750000981, 10.69163855873950020 ) ) ;
#10730 = EDGE_CURVE ( 'NONE', #2349, #6004, #2393, .T. ) ;
#10731 = LINE ( 'NONE', #1630, #5186 ) ;
#10732 = CARTESIAN_POINT ( 'NONE',  ( -71.99927362086853577, 76.65063509461015201, 12.50000000000143352 ) ) ;
#10733 = CARTESIAN_POINT ( 'NONE',  ( 11.24060940615075488, 54.98030487590998661, 0.01734873002535425313 ) ) ;
#10734 = AXIS2_PLACEMENT_3D ( 'NONE', #2525, #3300, #3353 ) ;
#10735 = CARTESIAN_POINT ( 'NONE',  ( -75.00000000000001421, 41.64360328783618570, 21.18013987092516359 ) ) ;
#10736 = ORIENTED_EDGE ( 'NONE', *, *, #10001, .T. ) ;
#10737 = CARTESIAN_POINT ( 'NONE',  ( -80.00000000000002842, 46.51471862576140381, 1.500003371917798756 ) ) ;
#10738 =( BOUNDED_CURVE ( )  B_SPLINE_CURVE ( 2, ( #5463, #892, #3665, #7330, #2533, #10955, #6426, #8941, #1571 ),
 .UNSPECIFIED., .F., .T. ) 
 B_SPLINE_CURVE_WITH_KNOTS ( ( 3, 2, 2, 2, 3 ),
 ( 0.07919667986333785159, 0.09899957127346223351, 0.1188024626835866154, 0.1386053540937109974, 0.1584082455038353654 ),
 .UNSPECIFIED. ) 
 CURVE ( )  GEOMETRIC_REPRESENTATION_ITEM ( )  RATIONAL_B_SPLINE_CURVE ( ( 0.9999999999999998890, 0.9238795325112866275, 0.9999999999999998890, 0.9238795325112866275, 0.9999999999999998890, 0.9238795325112866275, 0.9999999999999998890, 0.9238795325113071666, 0.9999999999999793499 ) ) 
 REPRESENTATION_ITEM ( '' )  );
#10739 = CARTESIAN_POINT ( 'NONE',  ( -70.34104699118842063, 33.99562393659818582, 0.006612473344882202446 ) ) ;
#10740 = ORIENTED_EDGE ( 'NONE', *, *, #2304, .T. ) ;
#10741 = CARTESIAN_POINT ( 'NONE',  ( -54.21479381498274108, 73.03707320332732422, 10.81077985938301822 ) ) ;
#10742 = CARTESIAN_POINT ( 'NONE',  ( -46.73803912521919557, 63.91895867764292660, -10.86094668994167023 ) ) ;
#10743 = CARTESIAN_POINT ( 'NONE',  ( -76.15625000204838102, 80.81189881250000440, -1.580522963032174394E-15 ) ) ;
#10744 = VERTEX_POINT ( 'NONE', #2458 ) ;
#10745 = CARTESIAN_POINT ( 'NONE',  ( -77.00000000204838102, 29.18810118750000981, 10.69163855873950020 ) ) ;
#10746 = DIRECTION ( 'NONE',  ( 0.000000000000000000, 0.000000000000000000, 1.000000000000000000 ) ) ;
#10747 = ORIENTED_EDGE ( 'NONE', *, *, #11621, .T. ) ;
#10748 = CARTESIAN_POINT ( 'NONE',  ( 0.000000000000000000, 0.000000000000000000, -4.696360911962001339 ) ) ;
#10749 = CARTESIAN_POINT ( 'NONE',  ( 10.98755190560986961, 51.02739634541043046, 3.053971085653802486 ) ) ;
#10750 = CARTESIAN_POINT ( 'NONE',  ( 1.576338153721813740, 55.00586181284610632, 0.002877765224681509519 ) ) ;
#10751 = ORIENTED_EDGE ( 'NONE', *, *, #236, .T. ) ;
#10752 = CARTESIAN_POINT ( 'NONE',  ( -11.47759590222061021, 75.47256375259368610, -5.508258824058441583 ) ) ;
#10753 = CARTESIAN_POINT ( 'NONE',  ( -32.99614454614441428, 33.97685596767119165, 0.0005149883856687357403 ) ) ;
#10754 = DIRECTION ( 'NONE',  ( 0.000000000000000000, -1.000000000000000000, 0.000000000000000000 ) ) ;
#10755 = CARTESIAN_POINT ( 'NONE',  ( 2.500000000000000000, 0.000000000000000000, -2.103846626247716234 ) ) ;
#10756 = CARTESIAN_POINT ( 'NONE',  ( -80.00000000000001421, 67.72792206135787296, 11.22792543327562775 ) ) ;
#10757 = EDGE_CURVE ( 'NONE', #5487, #4040, #10854, .T. ) ;
#10758 = ORIENTED_EDGE ( 'NONE', *, *, #5953, .T. ) ;
#10759 = CARTESIAN_POINT ( 'NONE',  ( -74.09375000409676204, 80.00000000000001421, -10.35533905932737753 ) ) ;
#10760 = DIRECTION ( 'NONE',  ( -1.000000000000000000, 0.000000000000000000, 0.000000000000000000 ) ) ;
#10761 = CARTESIAN_POINT ( 'NONE',  ( -15.00000000000000000, 55.00000000000000000, 20.00000000000000000 ) ) ;
#10762 = CARTESIAN_POINT ( 'NONE',  ( -59.88037020503378471, 51.91452991566635689, 20.80113349088246011 ) ) ;
#10763 = ORIENTED_EDGE ( 'NONE', *, *, #1253, .F. ) ;
#10764 = CARTESIAN_POINT ( 'NONE',  ( -78.00000000000001421, 46.51471862576140381, -8.485278002320759683 ) ) ;
#10765 = ADVANCED_FACE ( 'NONE', ( #357 ), #4023, .F. ) ;
#10766 = CARTESIAN_POINT ( 'NONE',  ( -78.78125000409680467, 65.35533905932737753, -24.99999999999999645 ) ) ;
#10767 = EDGE_CURVE ( 'NONE', #5641, #9755, #7244, .T. ) ;
#10768 = ORIENTED_EDGE ( 'NONE', *, *, #6551, .F. ) ;
#10769 = CARTESIAN_POINT ( 'NONE',  ( -2.500000000000000000, 3.061616997868383141E-16, -6.099999999999999645 ) ) ;
#10770 = CARTESIAN_POINT ( 'NONE',  ( 13.29588712016585106, 55.33163179650340169, 5.000002229370401174 ) ) ;
#10771 = CARTESIAN_POINT ( 'NONE',  ( -75.59375000204839523, 36.74823131438026280, 18.25176868561974786 ) ) ;
#10772 = DIRECTION ( 'NONE',  ( 0.000000000000000000, 0.000000000000000000, 1.000000000000000000 ) ) ;
#10773 = EDGE_LOOP ( 'NONE', ( #7466, #4056, #10102, #10864 ) ) ;
#10774 = DIRECTION ( 'NONE',  ( -0.000000000000000000, -1.000000000000000000, -0.000000000000000000 ) ) ;
#10775 = ORIENTED_EDGE ( 'NONE', *, *, #2024, .T. ) ;
#10776 = CARTESIAN_POINT ( 'NONE',  ( 13.04220382236630726, 70.42307724981912997, 19.68376297946718267 ) ) ;
#10777 = CARTESIAN_POINT ( 'NONE',  ( 19.12717080529655078, 62.03996031863259475, 12.21087854330282951 ) ) ;
#10778 = AXIS2_PLACEMENT_3D ( 'NONE', #9457, #10520, #465 ) ;
#10779 = DIRECTION ( 'NONE',  ( 0.000000000000000000, 0.000000000000000000, -1.000000000000000000 ) ) ;
#10780 = CARTESIAN_POINT ( 'NONE',  ( 5.000000000000000000, 2.886751345948134428, -5.653418012614792154 ) ) ;
#10781 = FACE_OUTER_BOUND ( 'NONE', #11342, .T. ) ;
#10782 = LINE ( 'NONE', #11564, #6152 ) ;
#10783 = ORIENTED_EDGE ( 'NONE', *, *, #5065, .T. ) ;
#10784 = PRESENTATION_STYLE_ASSIGNMENT (( #8163 ) ) ;
#10785 = CARTESIAN_POINT ( 'NONE',  ( -74.09375000204839523, 55.00000000000000000, 25.81189881249999729 ) ) ;
#10786 = EDGE_CURVE ( 'NONE', #6890, #1664, #11810, .T. ) ;
#10787 = DIRECTION ( 'NONE',  ( -1.000000000000000000, -0.000000000000000000, -0.000000000000000000 ) ) ;
#10788 = CARTESIAN_POINT ( 'NONE',  ( -77.09375000409677625, 80.00000000000001421, -10.35533905932737753 ) ) ;
#10789 = CARTESIAN_POINT ( 'NONE',  ( 7.335481199539121810, 54.99686737186916474, -0.0001706956380964400033 ) ) ;
#10790 = DIRECTION ( 'NONE',  ( 0.000000000000000000, 0.000000000000000000, 1.000000000000000000 ) ) ;
#10791 = CARTESIAN_POINT ( 'NONE',  ( -74.99999999999998579, 32.59534436559583526, -12.65407985245519917 ) ) ;
#10792 = ORIENTED_EDGE ( 'NONE', *, *, #6593, .T. ) ;
#10793 = DIRECTION ( 'NONE',  ( 0.8660254037844380415, -0.5000000000000009992, 0.000000000000000000 ) ) ;
#10794 = LINE ( 'NONE', #3442, #3264 ) ;
#10795 = VERTEX_POINT ( 'NONE', #5277 ) ;
#10796 = CARTESIAN_POINT ( 'NONE',  ( -22.39182375099971267, 57.05917196451265028, 20.98466401600494891 ) ) ;
#10797 = CARTESIAN_POINT ( 'NONE',  ( -77.65625000204838102, 80.81189881250000440, -1.580522963032174394E-15 ) ) ;
#10798 = VECTOR ( 'NONE', #6203, 1000.000000000000000 ) ;
#10799 = ORIENTED_EDGE ( 'NONE', *, *, #11404, .T. ) ;
#10800 = EDGE_CURVE ( 'NONE', #11066, #11373, #4559, .T. ) ;
#10801 = CARTESIAN_POINT ( 'NONE',  ( -71.59560441993426139, 80.81189881250000440, 6.916273537586018705 ) ) ;
#10802 = CARTESIAN_POINT ( 'NONE',  ( -78.00000000000001421, 63.48528137423857487, 6.985284746156351865 ) ) ;
#10803 =( BOUNDED_SURFACE ( )  B_SPLINE_SURFACE ( 1, 2, ( 
 ( #8153, #1849, #1011, #7441, #6370, #2878, #9277, #949, #168, #4735, #1910, #1738, #4671, #10109, #2815, #8324, #4614, #10895, #105, #6483, #1069, #3600, #2760, #8270, #9996, #3773, #2642, #827, #44, #5458, #6421, #6308, #11067, #6545, #9942, #5517, #8390, #3839, #5403, #3712, #7376, #9106, #2704, #10835, #9051, #4500, #886, #11794, #4561, #8212, #7265, #11847, #3658, #10950, #10051, #11003, #6844, #10414, #8510, #9341, #9401, #292, #6785, #2028, #2090, #4919, #4860, #6727, #2214, #5764, #3955, #5703, #2997, #9583, #3897, #8632, #4980, #2154, #3056, #5880, #11184, #7617, #9523, #9463, #4797, #1196, #10357 ),
 ( #8571, #3174, #10234, #5825, #11245, #5942, #7560, #350, #10468, #1129, #1249, #1313, #4077, #412, #10296, #2268, #4016, #7674, #8453, #11309, #3119, #6666, #11365, #5041, #7734, #1379, #8688, #470, #6607, #7503, #233, #11127, #2941, #7910, #5270, #1549, #6960, #5153, #8807, #4371, #584, #1434, #8744, #8023, #2385, #2450, #3472, #9638, #527, #699, #11539, #10759, #6061, #8917, #4305, #9696, #6898, #11421, #5098, #11661, #4190, #5214, #7963, #6116, #4251, #10527, #4127, #7850, #7137, #2335, #6005, #1603, #11479, #3290, #1493, #10702, #2568, #2515, #8864, #6235, #644, #9865, #9750, #3343, #10585, #11599, #3404 ) ),
 .UNSPECIFIED., .F., .F., .T. ) 
 B_SPLINE_SURFACE_WITH_KNOTS ( ( 2, 2 ),
 ( 3, 2, 2, 2, 2, 2, 2, 2, 2, 2, 2, 2, 2, 2, 2, 2, 2, 2, 2, 2, 2, 2, 2, 2, 2, 2, 2, 2, 2, 2, 2, 2, 2, 2, 2, 2, 2, 2, 2, 2, 2, 2, 2, 3 ),
 ( 0.000000000000000000, 1.000000000000000000 ),
 ( 0.000000000000000000, 0.02083333333333333218, 0.04166666666666666435, 0.06250000000000000000, 0.08333333333333332871, 0.1041666666666666713, 0.1250000000000000000, 0.1458333333333333426, 0.1666666666666666574, 0.1875000000000000000, 0.2083333333333333426, 0.2291666666666666574, 0.2500000000000000000, 0.2708333333333333148, 0.2916666666666666852, 0.3125000000000000000, 0.3333333333333333148, 0.3541666666666666852, 0.3750000000000000000, 0.3958333333333333148, 0.4166666666666666852, 0.4375000000000000000, 0.4583333333333333148, 0.4791666666666666852, 0.5000000000000000000, 0.5208333333333333703, 0.5416666666666666297, 0.5625000000000000000, 0.5833333333333333703, 0.6041666666666666297, 0.6250000000000000000, 0.6458333333333333703, 0.6666666666666666297, 0.6875000000000000000, 0.7083333333333333703, 0.7291666666666666297, 0.7500000000000000000, 0.7708333333333333703, 0.7916666666666666297, 0.8125000000000000000, 0.8333333333333333703, 0.8541666666666666297, 0.8750000000000000000, 0.8888490476107191451 ),
 .UNSPECIFIED. ) 
 GEOMETRIC_REPRESENTATION_ITEM ( )  RATIONAL_B_SPLINE_SURFACE ( (
 ( 1.000000000000000000, 0.9238795325112867385, 1.000000000000000000, 0.9238795325112867385, 1.000000000000000000, 0.9238795325112867385, 1.000000000000000000, 0.9238795325112867385, 1.000000000000000000, 0.9238795325112867385, 1.000000000000000000, 0.9238795325112867385, 1.000000000000000000, 0.9238795325112867385, 1.000000000000000000, 0.9238795325112867385, 1.000000000000000000, 0.9238795325112867385, 1.000000000000000000, 0.9238795325112867385, 1.000000000000000000, 0.9238795325112867385, 1.000000000000000000, 0.9238795325112867385, 1.000000000000000000, 0.9238795325112867385, 1.000000000000000000, 0.9238795325112867385, 1.000000000000000000, 0.9238795325112867385, 1.000000000000000000, 0.9238795325112867385, 1.000000000000000000, 0.9238795325112867385, 1.000000000000000000, 0.9238795325112867385, 1.000000000000000000, 0.9238795325112867385, 1.000000000000000000, 0.9238795325112867385, 1.000000000000000000, 0.9238795325112867385, 1.000000000000000000, 0.9238795325112867385, 1.000000000000000000, 0.9238795325112867385, 1.000000000000000000, 0.9238795325112867385, 1.000000000000000000, 0.9238795325112867385, 1.000000000000000000, 0.9238795325112867385, 1.000000000000000000, 0.9238795325112867385, 1.000000000000000000, 0.9238795325112867385, 1.000000000000000000, 0.9238795325112867385, 1.000000000000000000, 0.9238795325112867385, 1.000000000000000000, 0.9238795325112867385, 1.000000000000000000, 0.9238795325112867385, 1.000000000000000000, 0.9238795325112867385, 1.000000000000000000, 0.9238795325112867385, 1.000000000000000000, 0.9238795325112867385, 1.000000000000000000, 0.9238795325112867385, 1.000000000000000000, 0.9238795325112867385, 1.000000000000000000, 0.9238795325112867385, 1.000000000000000000, 0.9238795325112867385, 1.000000000000000000, 0.9238795325112867385, 1.000000000000000000, 0.9238795325112867385, 1.000000000000000000, 0.9238795325112867385, 1.000000000000000000, 0.9493985930367334625, 0.9660721903170175207),
 ( 1.000000000000000000, 0.9238795325112867385, 1.000000000000000000, 0.9238795325112867385, 1.000000000000000000, 0.9238795325112867385, 1.000000000000000000, 0.9238795325112867385, 1.000000000000000000, 0.9238795325112867385, 1.000000000000000000, 0.9238795325112867385, 1.000000000000000000, 0.9238795325112867385, 1.000000000000000000, 0.9238795325112867385, 1.000000000000000000, 0.9238795325112867385, 1.000000000000000000, 0.9238795325112867385, 1.000000000000000000, 0.9238795325112867385, 1.000000000000000000, 0.9238795325112867385, 1.000000000000000000, 0.9238795325112867385, 1.000000000000000000, 0.9238795325112867385, 1.000000000000000000, 0.9238795325112867385, 1.000000000000000000, 0.9238795325112867385, 1.000000000000000000, 0.9238795325112867385, 1.000000000000000000, 0.9238795325112867385, 1.000000000000000000, 0.9238795325112867385, 1.000000000000000000, 0.9238795325112867385, 1.000000000000000000, 0.9238795325112867385, 1.000000000000000000, 0.9238795325112867385, 1.000000000000000000, 0.9238795325112867385, 1.000000000000000000, 0.9238795325112867385, 1.000000000000000000, 0.9238795325112867385, 1.000000000000000000, 0.9238795325112867385, 1.000000000000000000, 0.9238795325112867385, 1.000000000000000000, 0.9238795325112867385, 1.000000000000000000, 0.9238795325112867385, 1.000000000000000000, 0.9238795325112867385, 1.000000000000000000, 0.9238795325112867385, 1.000000000000000000, 0.9238795325112867385, 1.000000000000000000, 0.9238795325112867385, 1.000000000000000000, 0.9238795325112867385, 1.000000000000000000, 0.9238795325112867385, 1.000000000000000000, 0.9238795325112867385, 1.000000000000000000, 0.9238795325112867385, 1.000000000000000000, 0.9238795325112867385, 1.000000000000000000, 0.9238795325112867385, 1.000000000000000000, 0.9238795325112867385, 1.000000000000000000, 0.9238795325112867385, 1.000000000000000000, 0.9238795325112867385, 1.000000000000000000, 0.9493985930367334625, 0.9660721903170175207) ) ) 
 REPRESENTATION_ITEM ( '' )  SURFACE ( )  );
#10804 = DIRECTION ( 'NONE',  ( 0.000000000000000000, 1.000000000000000000, 0.000000000000000000 ) ) ;
#10805 = ADVANCED_FACE ( 'NONE', ( #9046 ), #11609, .F. ) ;
#10806 = CARTESIAN_POINT ( 'NONE',  ( 9.573972992054704534, 54.99220333846943021, 0.01448963470816768892 ) ) ;
#10807 = VECTOR ( 'NONE', #3042, 1000.000000000000000 ) ;
#10808 = ORIENTED_EDGE ( 'NONE', *, *, #8958, .F. ) ;
#10809 = CARTESIAN_POINT ( 'NONE',  ( 13.47757237172695000, 49.50866688550052430, 20.43174547745228864 ) ) ;
#10810 = CARTESIAN_POINT ( 'NONE',  ( -39.18898618735786243, 44.43394377878069434, -18.33326528472845141 ) ) ;
#10811 = LINE ( 'NONE', #1655, #2374 ) ;
#10812 = LINE ( 'NONE', #5267, #8027 ) ;
#10813 = APPLICATION_CONTEXT ( 'automotive_design' ) ;
#10814 = DIRECTION ( 'NONE',  ( -1.000000000000000000, 0.000000000000000000, 0.000000000000000000 ) ) ;
#10815 = EDGE_CURVE ( 'NONE', #8716, #11173, #6363, .T. ) ;
#10816 = ORIENTED_EDGE ( 'NONE', *, *, #1799, .F. ) ;
#10817 = DIRECTION ( 'NONE',  ( 8.659560562354974766E-17, -0.7071067811865441310, 0.7071067811865507924 ) ) ;
#10818 = CYLINDRICAL_SURFACE ( 'NONE', #11451, 1.499999999999999556 ) ;
#10819 = DIRECTION ( 'NONE',  ( 0.000000000000000000, -0.000000000000000000, -1.000000000000000000 ) ) ;
#10820 = AXIS2_PLACEMENT_3D ( 'NONE', #11389, #3200, #2063 ) ;
#10821 = CARTESIAN_POINT ( 'NONE',  ( -66.81799029952708224, 34.52069382205590387, 5.503409927558503334 ) ) ;
#10822 = ORIENTED_EDGE ( 'NONE', *, *, #2216, .F. ) ;
#10823 = CARTESIAN_POINT ( 'NONE',  ( -80.00000000000001421, 54.99999999999999289, -15.47055937655931501 ) ) ;
#10824 = PRODUCT ( 'Internal Tapered Feed Screw Auger', 'Internal Tapered Feed Screw Auger', '', ( #2829 ) ) ;
#10825 = CONICAL_SURFACE ( 'NONE', #876, 2.999999999999995559, 0.7853981633974420618 ) ;
#10826 = CARTESIAN_POINT ( 'NONE',  ( -63.31773346265211444, 53.70568493644218933, 4.840560537982487865 ) ) ;
#10827 = B_SPLINE_CURVE_WITH_KNOTS ( 'NONE', 3,
 ( #4517, #1700, #10011, #732, #9015, #1806, #9960, #5474, #9122, #8214, #2644, #1912, #9165, #951, #2708, #6310, #6254, #5346, #774, #10952, #8272, #1741, #9998, #8999, #10837, #4450, #11849, #11679, #3539, #8103, #46, #5405, #8041, #4617, #3714, #9882 ),
 .UNSPECIFIED., .F., .F.,
 ( 4, 2, 2, 2, 2, 2, 2, 2, 2, 2, 2, 2, 2, 2, 2, 2, 2, 4 ),
 ( 0.07284642870127019942, 0.07360525742480880651, 0.07436408614834741360, 0.07588174359542464165, 0.07739940104250185582, 0.07891705848957906999, 0.08043471593665629804, 0.08195237338373351221, 0.08347003083081072639, 0.08498768827788795444, 0.08574651700142656152, 0.08650534572496516861, 0.08802300317204239666, 0.08954066061911961083, 0.09105831806619682500, 0.09257597551327405305, 0.09409363296035126722, 0.09712894785450570945 ),
 .UNSPECIFIED. ) ;
#10828 = ORIENTED_EDGE ( 'NONE', *, *, #8050, .T. ) ;
#10829 = CARTESIAN_POINT ( 'NONE',  ( -78.00000000000001421, 63.48528137423857487, 3.371917795327861178E-06 ) ) ;
#10830 = CARTESIAN_POINT ( 'NONE',  ( 17.95684494300012801, 58.76662442904990513, 3.304478729834980921 ) ) ;
#10831 = CARTESIAN_POINT ( 'NONE',  ( -74.65625000204838102, 80.81189881250000440, -1.580522963032174394E-15 ) ) ;
#10832 = CARTESIAN_POINT ( 'NONE',  ( -77.93750000204838102, 65.69163855873948421, -25.81189881250000440 ) ) ;
#10833 = VERTEX_POINT ( 'NONE', #10944 ) ;
#10834 = VECTOR ( 'NONE', #2341, 1000.000000000000000 ) ;
#10835 = CARTESIAN_POINT ( 'NONE',  ( -75.31250000204839523, 29.18810118750000981, 10.69163855873950020 ) ) ;
#10836 = ORIENTED_EDGE ( 'NONE', *, *, #1525, .T. ) ;
#10837 = CARTESIAN_POINT ( 'NONE',  ( -0.2902744515997993657, 53.38936837472795816, -4.744839395679999683 ) ) ;
#10838 = AXIS2_PLACEMENT_3D ( 'NONE', #5453, #9047, #7371 ) ;
#10839 = CARTESIAN_POINT ( 'NONE',  ( 6.664798253476140744, 40.98022014747188990, -0.0003427094624634590900 ) ) ;
#10840 = CARTESIAN_POINT ( 'NONE',  ( -78.21875000204839523, 29.18810118750000271, 4.741568889096522788E-15 ) ) ;
#10841 = CARTESIAN_POINT ( 'NONE',  ( 2.500000000000000000, 0.000000000000000000, -0.3755037691048591086 ) ) ;
#10842 = CARTESIAN_POINT ( 'NONE',  ( 2.400054171417768487E-15, 64.99605696851786263, -19.59792961213366169 ) ) ;
#10843 = VECTOR ( 'NONE', #5994, 1000.000000000000114 ) ;
#10844 = CARTESIAN_POINT ( 'NONE',  ( -74.09375000204839523, 36.74823131438026280, 18.25176868561974786 ) ) ;
#10845 = COLOUR_RGB ( '',0.8941176470588234615, 0.8941176470588234615, 0.8941176470588234615 ) ;
#10846 = EDGE_LOOP ( 'NONE', ( #6013, #7212, #2082, #5475 ) ) ;
#10847 = ADVANCED_FACE ( 'NONE', ( #6303 ), #5397, .T. ) ;
#10848 =( NAMED_UNIT ( * ) SI_UNIT ( $, .STERADIAN. ) SOLID_ANGLE_UNIT ( ) );
#10849 = CARTESIAN_POINT ( 'NONE',  ( -76.15625000409677625, 30.00000000000000355, -10.35533905932738108 ) ) ;
#10850 = DIRECTION ( 'NONE',  ( -1.000000000000000000, -0.000000000000000000, -0.000000000000000000 ) ) ;
#10851 = DIRECTION ( 'NONE',  ( 0.000000000000000000, 0.000000000000000000, 1.000000000000000000 ) ) ;
#10852 = CARTESIAN_POINT ( 'NONE',  ( -39.33118544708877096, 55.00017070458616786, -0.003132656074481668385 ) ) ;
#10853 = SHAPE_DEFINITION_REPRESENTATION ( #6920, #9454 ) ;
#10854 = CIRCLE ( 'NONE', #530, 22.00000000000000000 ) ;
#10855 = CARTESIAN_POINT ( 'NONE',  ( -15.83487696431883762, 72.27984571272472181, -13.62867557726837475 ) ) ;
#10856 = CARTESIAN_POINT ( 'NONE',  ( -25.95462006380511966, 51.23402121196087933, 3.305273135093794501 ) ) ;
#10857 = LINE ( 'NONE', #7286, #8815 ) ;
#10858 = VERTEX_POINT ( 'NONE', #9990 ) ;
#10859 = CARTESIAN_POINT ( 'NONE',  ( -29.69731012496106359, 35.99954121986550604, 8.986476355089152435 ) ) ;
#10860 = CARTESIAN_POINT ( 'NONE',  ( -75.78125000204838102, 55.00000000000000000, 25.81189881249999729 ) ) ;
#10861 = ORIENTED_EDGE ( 'NONE', *, *, #8165, .F. ) ;
#10862 = CARTESIAN_POINT ( 'NONE',  ( -76.71875000000004263, 79.99999999999990052, -10.35533905932733667 ) ) ;
#10863 = CARTESIAN_POINT ( 'NONE',  ( 2.826857198123298165, 37.44742646213195769, -11.71858918393001225 ) ) ;
#10864 = ORIENTED_EDGE ( 'NONE', *, *, #365, .T. ) ;
#10865 = DIRECTION ( 'NONE',  ( 0.000000000000000000, 0.000000000000000000, -1.000000000000000000 ) ) ;
#10866 = CARTESIAN_POINT ( 'NONE',  ( 0.9978688846961245584, 55.00160005685901865, 0.0008981051542724318056 ) ) ;
#10867 = VERTEX_POINT ( 'NONE', #880 ) ;
#10868 = CARTESIAN_POINT ( 'NONE',  ( 6.839732782626861685, 34.30800418419381259, 4.109398041371060017 ) ) ;
#10869 = CARTESIAN_POINT ( 'NONE',  ( -7.030643242133587378, 62.08114452727563304, -19.79025909736091648 ) ) ;
#10870 = CARTESIAN_POINT ( 'NONE',  ( 5.000000000000000888, 0.000000000000000000, -6.099999999999999645 ) ) ;
#10871 = CIRCLE ( 'NONE', #2274, 1.500000000000001332 ) ;
#10872 = DIRECTION ( 'NONE',  ( -1.000000000000000000, 0.000000000000000000, 0.000000000000000000 ) ) ;
#10873 = CARTESIAN_POINT ( 'NONE',  ( 2.500000000000000000, 0.000000000000000000, -4.696360911962001339 ) ) ;
#10874 = VERTEX_POINT ( 'NONE', #7259 ) ;
#10875 = EDGE_CURVE ( 'NONE', #10958, #6384, #10663, .T. ) ;
#10876 = FACE_OUTER_BOUND ( 'NONE', #11478, .T. ) ;
#10877 = CARTESIAN_POINT ( 'NONE',  ( -20.87154949818722116, 55.00167759324021688, 0.002033656601463836207 ) ) ;
#10878 = CARTESIAN_POINT ( 'NONE',  ( -56.29331228730723069, 56.60826288146544272, 4.745686675311040048 ) ) ;
#10879 = EDGE_CURVE ( 'NONE', #10459, #3494, #1670, .T. ) ;
#10880 = CIRCLE ( 'NONE', #554, 1.500000000000001332 ) ;
#10881 = ORIENTED_EDGE ( 'NONE', *, *, #4904, .T. ) ;
#10882 = CARTESIAN_POINT ( 'NONE',  ( -74.75000000000000000, 55.00000000000000000, 24.99999999999999645 ) ) ;
#10883 = AXIS2_PLACEMENT_3D ( 'NONE', #5329, #7964, #7191 ) ;
#10884 = CARTESIAN_POINT ( 'NONE',  ( -67.20012888935585238, 51.02918010271523030, 3.055874726862140900 ) ) ;
#10885 = EDGE_CURVE ( 'NONE', #3293, #3451, #6189, .T. ) ;
#10886 = VERTEX_POINT ( 'NONE', #9935 ) ;
#10887 = DIRECTION ( 'NONE',  ( 0.000000000000000000, 1.000000000000000000, 0.000000000000000000 ) ) ;
#10888 = APPLICATION_CONTEXT ( 'automotive_design' ) ;
#10889 = CARTESIAN_POINT ( 'NONE',  ( 0.000000000000000000, 0.000000000000000000, -3.832189483390572970 ) ) ;
#10890 = FACE_OUTER_BOUND ( 'NONE', #7824, .T. ) ;
#10891 = CARTESIAN_POINT ( 'NONE',  ( -74.46875000204839523, 73.25176868561975141, 18.25176868561974075 ) ) ;
#10892 = CARTESIAN_POINT ( 'NONE',  ( -78.03125000204838102, 55.00000000000000000, -25.81189881249999729 ) ) ;
#10893 = VECTOR ( 'NONE', #1564, 1000.000000000000000 ) ;
#10894 = ORIENTED_EDGE ( 'NONE', *, *, #9085, .F. ) ;
#10895 = CARTESIAN_POINT ( 'NONE',  ( -77.75000000204839523, 65.69163855873948421, -25.81189881250000440 ) ) ;
#10896 = VERTEX_POINT ( 'NONE', #708 ) ;
#10897 = CARTESIAN_POINT ( 'NONE',  ( 22.02083420892270382, 77.24169289693605833, 11.42124585519064972 ) ) ;
#10898 = CARTESIAN_POINT ( 'NONE',  ( -26.59538538879835556, 44.11636033083960484, 8.941403297748980350 ) ) ;
#10899 = CARTESIAN_POINT ( 'NONE',  ( -77.37500000204838102, 80.81189881250000440, 10.69163855873948243 ) ) ;
#10900 = CARTESIAN_POINT ( 'NONE',  ( -76.71875000409676204, 65.35533905932729226, 25.00000000000008527 ) ) ;
#10901 = AXIS2_PLACEMENT_3D ( 'NONE', #7581, #2901, #9423 ) ;
#10902 = ADVANCED_FACE ( 'NONE', ( #6413 ), #535, .F. ) ;
#10903 = CARTESIAN_POINT ( 'NONE',  ( -78.12500000000004263, 79.99999999999992895, -1.530808498934187183E-15 ) ) ;
#10904 = ORIENTED_EDGE ( 'NONE', *, *, #2571, .F. ) ;
#10905 = VECTOR ( 'NONE', #2010, 1000.000000000000000 ) ;
#10906 = CARTESIAN_POINT ( 'NONE',  ( 0.000000000000000000, 0.000000000000000000, -0.5394676594665810399 ) ) ;
#10907 = CARTESIAN_POINT ( 'NONE',  ( -72.31250000204839523, 29.18810118750000981, 10.69163855873950020 ) ) ;
#10908 = CYLINDRICAL_SURFACE ( 'NONE', #1183, 1.499999999999999556 ) ;
#10909 = EDGE_CURVE ( 'NONE', #6890, #7832, #3412, .T. ) ;
#10910 = ADVANCED_FACE ( 'NONE', ( #7202 ), #9819, .F. ) ;
#10911 = CARTESIAN_POINT ( 'NONE',  ( -30.00213106679868957, 55.00296086862838507, 0.0002306145982448079112 ) ) ;
#10912 = CARTESIAN_POINT ( 'NONE',  ( -3.611159399822559735, 65.46779913315577915, -19.35030201487227330 ) ) ;
#10913 = AXIS2_PLACEMENT_3D ( 'NONE', #7381, #49, #8105 ) ;
#10914 = DIRECTION ( 'NONE',  ( -1.000000000000000000, 0.000000000000000000, 0.000000000000000000 ) ) ;
#10915 = ORIENTED_EDGE ( 'NONE', *, *, #197, .T. ) ;
#10916 = CARTESIAN_POINT ( 'NONE',  ( -63.63584090060282961, 46.00639722032484968, 19.01118640546643590 ) ) ;
#10917 = EDGE_CURVE ( 'NONE', #4670, #7593, #1842, .T. ) ;
#10918 = VERTEX_POINT ( 'NONE', #3593 ) ;
#10919 = CARTESIAN_POINT ( 'NONE',  ( 1.697306494461763959, 35.98764835359665426, -8.991780390316415961 ) ) ;
#10920 = CARTESIAN_POINT ( 'NONE',  ( -73.71875000204839523, 36.74823131438024859, -18.25176868561973720 ) ) ;
#10921 = VECTOR ( 'NONE', #6531, 1000.000000000000000 ) ;
#10922 = AXIS2_PLACEMENT_3D ( 'NONE', #1560, #4318, #1501 ) ;
#10923 = ORIENTED_EDGE ( 'NONE', *, *, #2723, .F. ) ;
#10924 = CARTESIAN_POINT ( 'NONE',  ( -71.44842626887532333, 72.99142816090481745, 20.46173487478911568 ) ) ;
#10925 = CARTESIAN_POINT ( 'NONE',  ( -17.88142570751413274, 67.52739394234649239, 16.89079266652326439 ) ) ;
#10926 = ORIENTED_EDGE ( 'NONE', *, *, #7423, .T. ) ;
#10927 = LINE ( 'NONE', #8907, #10307 ) ;
#10928 = VECTOR ( 'NONE', #840, 1000.000000000000000 ) ;
#10929 = CARTESIAN_POINT ( 'NONE',  ( -10.66879778189107419, 54.99855794386581209, 0.001134569799796503100 ) ) ;
#10930 = ORIENTED_EDGE ( 'NONE', *, *, #11161, .F. ) ;
#10931 = CARTESIAN_POINT ( 'NONE',  ( -59.67156972769491574, 55.00060627355243525, 21.02858942331178227 ) ) ;
#10932 = CARTESIAN_POINT ( 'NONE',  ( -19.59602372284622618, 68.34451306940553650, 16.25656885606184332 ) ) ;
#10933 = CARTESIAN_POINT ( 'NONE',  ( 1.648146632868999095, 4.821944789745366222, -6.100000000000003197 ) ) ;
#10934 = PLANE ( 'NONE',  #6211 ) ;
#10935 = FACE_OUTER_BOUND ( 'NONE', #6933, .T. ) ;
#10936 = DIRECTION ( 'NONE',  ( -1.000000000000000000, -0.000000000000000000, -0.000000000000000000 ) ) ;
#10937 = VERTEX_POINT ( 'NONE', #8032 ) ;
#10938 = CARTESIAN_POINT ( 'NONE',  ( -76.71875000000004263, 79.99999999999990052, -10.35533905932733667 ) ) ;
#10939 = CARTESIAN_POINT ( 'NONE',  ( -53.83687749268464984, 54.99647651120280045, -0.001734407420701496736 ) ) ;
#10940 = CARTESIAN_POINT ( 'NONE',  ( -59.02007697189144153, 54.33745946848893738, 5.000024639461678966 ) ) ;
#10941 = FACE_OUTER_BOUND ( 'NONE', #9126, .T. ) ;
#10942 = LINE ( 'NONE', #4004, #9130 ) ;
#10943 = VERTEX_POINT ( 'NONE', #2579 ) ;
#10944 = CARTESIAN_POINT ( 'NONE',  ( -77.37500000409677625, 55.00000000000000000, -24.99999999999999645 ) ) ;
#10945 = CYLINDRICAL_SURFACE ( 'NONE', #3074, 1.500000000000000000 ) ;
#10946 = CARTESIAN_POINT ( 'NONE',  ( 16.01486940960983674, 57.50823208304175438, 4.337747975045839866 ) ) ;
#10947 = CARTESIAN_POINT ( 'NONE',  ( -4.242132748603181014, 66.03411770982167184, -22.43350638257962615 ) ) ;
#10948 = CARTESIAN_POINT ( 'NONE',  ( -76.81250000204838102, 29.18810118750000626, -10.69163855873949309 ) ) ;
#10949 = ORIENTED_EDGE ( 'NONE', *, *, #913, .F. ) ;
#10950 = CARTESIAN_POINT ( 'NONE',  ( -74.37500000204838102, 80.81189881250001861, 10.69163855873948599 ) ) ;
#10951 = ORIENTED_EDGE ( 'NONE', *, *, #8504, .F. ) ;
#10952 = CARTESIAN_POINT ( 'NONE',  ( -2.043570261588242953, 54.83463289114614270, -4.999998501150977326 ) ) ;
#10953 = CARTESIAN_POINT ( 'NONE',  ( -20.73803862786483165, 56.37319242487460258, 13.98159745988486868 ) ) ;
#10954 = CARTESIAN_POINT ( 'NONE',  ( -75.31250000204839523, 29.18810118750000981, 10.69163855873950020 ) ) ;
#10955 = CARTESIAN_POINT ( 'NONE',  ( -78.78125000000002842, 30.00000000000003553, -10.35533905932737042 ) ) ;
#10956 = EDGE_CURVE ( 'NONE', #10179, #11278, #1785, .T. ) ;
#10957 = LINE ( 'NONE', #7272, #10477 ) ;
#10958 = VERTEX_POINT ( 'NONE', #7317 ) ;
#10959 = DIRECTION ( 'NONE',  ( -0.000000000000000000, -0.000000000000000000, -1.000000000000000000 ) ) ;
#10960 = CARTESIAN_POINT ( 'NONE',  ( -72.87500000204840944, 80.81189881250001861, 10.69163855873948599 ) ) ;
#10961 = DIRECTION ( 'NONE',  ( 0.000000000000000000, 0.000000000000000000, 1.000000000000000000 ) ) ;
#10962 = CARTESIAN_POINT ( 'NONE',  ( -58.87201974314975672, 55.00020036712756877, 0.003823789621534544932 ) ) ;
#10963 = CONTEXT_DEPENDENT_SHAPE_REPRESENTATION ( #5950, #8350 ) ;
#10964 = CARTESIAN_POINT ( 'NONE',  ( 36.99999999999999289, 55.00000000000000000, 0.000000000000000000 ) ) ;
#10965 = DIRECTION ( 'NONE',  ( -0.000000000000000000, -0.000000000000000000, -1.000000000000000000 ) ) ;
#10966 = ORIENTED_EDGE ( 'NONE', *, *, #7898, .T. ) ;
#10967 = EDGE_CURVE ( 'NONE', #9436, #19, #8872, .T. ) ;
#10968 = CARTESIAN_POINT ( 'NONE',  ( -78.00000000000001421, 54.99999999999998579, -9.985278002320759683 ) ) ;
#10969 = ORIENTED_EDGE ( 'NONE', *, *, #2171, .T. ) ;
#10970 = CARTESIAN_POINT ( 'NONE',  ( 21.47754340280339136, 75.43473409906381733, 5.492671141289128478 ) ) ;
#10971 = CARTESIAN_POINT ( 'NONE',  ( -78.40625000204839523, 36.74823131438026280, 18.25176868561974786 ) ) ;
#10972 = ORIENTED_EDGE ( 'NONE', *, *, #6827, .F. ) ;
#10973 = CARTESIAN_POINT ( 'NONE',  ( -76.25000000204838102, 80.81189881250001861, -10.69163855873949132 ) ) ;
#10974 = CARTESIAN_POINT ( 'NONE',  ( -5.337209886265139147, 63.04750289227570192, -19.42727033598380970 ) ) ;
#10975 = EDGE_CURVE ( 'NONE', #96, #4662, #4552, .T. ) ;
#10976 = ORIENTED_EDGE ( 'NONE', *, *, #4690, .F. ) ;
#10977 = DIRECTION ( 'NONE',  ( -0.000000000000000000, -0.000000000000000000, 1.000000000000000000 ) ) ;
#10978 = PRODUCT_DEFINITION_FORMATION_WITH_SPECIFIED_SOURCE ( 'ANY', '', #1453, .NOT_KNOWN. ) ;
#10979 = CARTESIAN_POINT ( 'NONE',  ( -58.16650030231640045, 58.91145824815324517, 5.848851387972111127 ) ) ;
#10980 = ORIENTED_EDGE ( 'NONE', *, *, #9896, .T. ) ;
#10981 = CARTESIAN_POINT ( 'NONE',  ( -41.00387659642365179, 55.00043089085527726, -21.02791246669550773 ) ) ;
#10982 = CARTESIAN_POINT ( 'NONE',  ( -23.05849041873830885, 57.05917197429855037, 20.98589082339331569 ) ) ;
#10983 = DIRECTION ( 'NONE',  ( -1.000000000000000000, -0.000000000000000000, -0.000000000000000000 ) ) ;
#10984 = FILL_AREA_STYLE ('',( #6289 ) ) ;
#10985 = CARTESIAN_POINT ( 'NONE',  ( -75.00000000000000000, 55.00000000000000000, 0.000000000000000000 ) ) ;
#10986 = CARTESIAN_POINT ( 'NONE',  ( -75.00000000000000000, 55.00000000000000000, -25.00000000000000355 ) ) ;
#10987 = VERTEX_POINT ( 'NONE', #11237 ) ;
#10988 = DIRECTION ( 'NONE',  ( 0.000000000000000000, 1.000000000000000000, 0.000000000000000000 ) ) ;
#10989 = CARTESIAN_POINT ( 'NONE',  ( -39.42605725089504176, 54.98959656231615156, -0.01274862175783714538 ) ) ;
#10990 = CARTESIAN_POINT ( 'NONE',  ( -59.79376487574317167, 53.69725619367564207, 4.871814158559260477 ) ) ;
#10991 = CIRCLE ( 'NONE', #6427, 2.500000000000000000 ) ;
#10992 = CARTESIAN_POINT ( 'NONE',  ( 36.99999999999999289, 55.00000000000000000, 0.000000000000000000 ) ) ;
#10993 = CARTESIAN_POINT ( 'NONE',  ( -75.12500000409677625, 55.00000000000000000, 24.99999999999999645 ) ) ;
#10994 = EDGE_LOOP ( 'NONE', ( #3661, #2455, #10758, #3565 ) ) ;
#10995 = EDGE_CURVE ( 'NONE', #5852, #9331, #6297, .T. ) ;
#10996 = CARTESIAN_POINT ( 'NONE',  ( -5.000000000000000888, 0.000000000000000000, 0.000000000000000000 ) ) ;
#10997 = CARTESIAN_POINT ( 'NONE',  ( -28.71241679207687625, 51.69383968972351795, 3.765155372993232330 ) ) ;
#10998 = DIRECTION ( 'NONE',  ( 1.000000000000000000, 0.000000000000000000, 0.000000000000000000 ) ) ;
#10999 = CARTESIAN_POINT ( 'NONE',  ( -6.643805856392553721, 66.86877144058414046, -22.00652157144978105 ) ) ;
#11000 = CARTESIAN_POINT ( 'NONE',  ( -78.40625000204838102, 29.18810118750000271, 4.741568889096522788E-15 ) ) ;
#11001 = AXIS2_PLACEMENT_3D ( 'NONE', #6111, #5208, #4121 ) ;
#11002 = ORIENTED_EDGE ( 'NONE', *, *, #11272, .F. ) ;
#11003 = CARTESIAN_POINT ( 'NONE',  ( -74.18750000204839523, 65.69163855873949842, 25.81189881250000440 ) ) ;
#11004 = ORIENTED_EDGE ( 'NONE', *, *, #8880, .F. ) ;
#11005 = CARTESIAN_POINT ( 'NONE',  ( 8.158495005360048680, 67.55745455422055556, 21.62097722686486279 ) ) ;
#11006 = CARTESIAN_POINT ( 'NONE',  ( -7.331473370266870404, 64.90913857603797510, -9.909739041900611056 ) ) ;
#11007 =( GEOMETRIC_REPRESENTATION_CONTEXT ( 3 ) GLOBAL_UNCERTAINTY_ASSIGNED_CONTEXT ( ( #1062 ) ) GLOBAL_UNIT_ASSIGNED_CONTEXT ( ( #8594, #5116, #3190 ) ) REPRESENTATION_CONTEXT ( 'NONE', 'WORKASPACE' ) );
#11008 = CARTESIAN_POINT ( 'NONE',  ( -77.28125000204839523, 73.25176868561975141, 18.25176868561974075 ) ) ;
#11009 = DIRECTION ( 'NONE',  ( 0.000000000000000000, 1.000000000000000000, 0.000000000000000000 ) ) ;
#11010 = CARTESIAN_POINT ( 'NONE',  ( 0.000000000000000000, 0.000000000000000000, -6.099999999999999645 ) ) ;
#11011 = ORIENTED_EDGE ( 'NONE', *, *, #7065, .T. ) ;
#11012 = EDGE_CURVE ( 'NONE', #6194, #1492, #2818, .T. ) ;
#11013 = CARTESIAN_POINT ( 'NONE',  ( -3.000000000000000888, 0.000000000000000000, -6.074599999999999334 ) ) ;
#11014 = CARTESIAN_POINT ( 'NONE',  ( -77.18750000409679046, 72.67766952966368876, -17.67766952966368876 ) ) ;
#11015 = CYLINDRICAL_SURFACE ( 'NONE', #7110, 1.499999999999999556 ) ;
#11016 = CARTESIAN_POINT ( 'NONE',  ( -21.42602701979682323, 54.99834091475071318, 0.02619292028802366196 ) ) ;
#11017 = APPLICATION_PROTOCOL_DEFINITION ( 'draft international standard', 'automotive_design', 1998, #10659 ) ;
#11018 = CARTESIAN_POINT ( 'NONE',  ( -6.986265722248286458, 66.68765601544015453, -18.64146191746018744 ) ) ;
#11019 = VECTOR ( 'NONE', #4116, 1000.000000000000000 ) ;
#11020 = CARTESIAN_POINT ( 'NONE',  ( -78.00000000000001421, 42.27207793864211283, -11.22791868944003824 ) ) ;
#11021 = AXIS2_PLACEMENT_3D ( 'NONE', #1061, #282, #7433 ) ;
#11022 = ORIENTED_EDGE ( 'NONE', *, *, #8576, .F. ) ;
#11023 = CARTESIAN_POINT ( 'NONE',  ( 8.071484979291650319, 50.06510116776722441, 0.8205671114678182443 ) ) ;
#11024 = EDGE_CURVE ( 'NONE', #3681, #2740, #5121, .T. ) ;
#11025 = DIRECTION ( 'NONE',  ( -1.000000000000000000, -0.000000000000000000, -0.000000000000000000 ) ) ;
#11026 = EDGE_CURVE ( 'NONE', #6771, #7713, #3776, .T. ) ;
#11027 = ORIENTED_EDGE ( 'NONE', *, *, #2950, .F. ) ;
#11028 = CARTESIAN_POINT ( 'NONE',  ( 15.18896243380506306, 60.50666922109576262, 20.46968130491651650 ) ) ;
#11029 = CARTESIAN_POINT ( 'NONE',  ( -77.28125000204839523, 73.25176868561975141, 18.25176868561974075 ) ) ;
#11030 = VERTEX_POINT ( 'NONE', #10996 ) ;
#11031 = DIRECTION ( 'NONE',  ( 9.813077866773612233E-16, -1.000000000000000000, -0.000000000000000000 ) ) ;
#11032 = CARTESIAN_POINT ( 'NONE',  ( -41.21475901749523274, 58.08538884819615333, -20.80179922188357011 ) ) ;
#11033 =( NAMED_UNIT ( * ) PLANE_ANGLE_UNIT ( ) SI_UNIT ( $, .RADIAN. ) );
#11034 = CARTESIAN_POINT ( 'NONE',  ( -38.60828084422895046, 48.85949782923615459, -20.20603288453101243 ) ) ;
#11035 = ORIENTED_EDGE ( 'NONE', *, *, #6539, .F. ) ;
#11036 = CARTESIAN_POINT ( 'NONE',  ( -72.12500000409677625, 55.00000000000000000, 24.99999999999999645 ) ) ;
#11037 = ADVANCED_FACE ( 'NONE', ( #3705 ), #5693, .F. ) ;
#11038 = CARTESIAN_POINT ( 'NONE',  ( 21.47754340280339136, 75.43473409906381733, 5.492671141289128478 ) ) ;
#11039 = AXIS2_PLACEMENT_3D ( 'NONE', #9113, #5523, #9171 ) ;
#11040 = ORIENTED_EDGE ( 'NONE', *, *, #3370, .F. ) ;
#11041 = ADVANCED_FACE ( 'NONE', ( #7551 ), #8724, .T. ) ;
#11042 = CARTESIAN_POINT ( 'NONE',  ( -52.67050196621227798, 74.42705245932049252, 8.047455632081089050 ) ) ;
#11043 = ADVANCED_FACE ( 'NONE', ( #3482 ), #1787, .F. ) ;
#11044 = CARTESIAN_POINT ( 'NONE',  ( -42.92935705524211443, 57.05913440163546113, -20.93112575922673102 ) ) ;
#11045 = CARTESIAN_POINT ( 'NONE',  ( -5.000000000000000888, -1.936377641173858466, -0.1973691732449216474 ) ) ;
#11046 = DIRECTION ( 'NONE',  ( -1.000000000000000000, 0.000000000000000000, 0.000000000000000000 ) ) ;
#11047 = CARTESIAN_POINT ( 'NONE',  ( -78.00000000000002842, 38.02943725152282184, 3.371917797929946392E-06 ) ) ;
#11048 = DIRECTION ( 'NONE',  ( 0.000000000000000000, 0.000000000000000000, -1.000000000000000000 ) ) ;
#11049 = B_SPLINE_CURVE_WITH_KNOTS ( 'NONE', 3,
 ( #6137, #1452, #4145, #4209 ),
 .UNSPECIFIED., .F., .F.,
 ( 4, 4 ),
 ( 2.380735200861166196E-07, 0.002921158011986710757 ),
 .UNSPECIFIED. ) ;
#11050 = EDGE_LOOP ( 'NONE', ( #1349, #170, #7888, #2691 ) ) ;
#11051 = CARTESIAN_POINT ( 'NONE',  ( 73.00000000000000000, 97.00000000000000000, -9.797174393178809880E-16 ) ) ;
#11052 = CARTESIAN_POINT ( 'NONE',  ( -57.33538960692911957, 54.99887155840742992, -0.001353544291193513891 ) ) ;
#11053 = CARTESIAN_POINT ( 'NONE',  ( -36.85275351908241959, 52.78708903700569977, -4.486665150141578629 ) ) ;
#11054 = EDGE_CURVE ( 'NONE', #10565, #6614, #4931, .T. ) ;
#11055 = ADVANCED_FACE ( 'NONE', ( #7261 ), #5893, .F. ) ;
#11056 = EDGE_CURVE ( 'NONE', #9462, #6597, #4556, .T. ) ;
#11057 = CARTESIAN_POINT ( 'NONE',  ( -74.37500000409677625, 55.00000000000000000, -24.99999999999999645 ) ) ;
#11058 = CARTESIAN_POINT ( 'NONE',  ( -61.33571477330379196, 55.00015097948840292, 14.01955991042104444 ) ) ;
#11059 = ORIENTED_EDGE ( 'NONE', *, *, #2201, .T. ) ;
#11060 = DIRECTION ( 'NONE',  ( -1.000000000000000000, -0.000000000000000000, -0.000000000000000000 ) ) ;
#11061 = CARTESIAN_POINT ( 'NONE',  ( -72.21875000204838102, 36.74823131438024859, -18.25176868561973720 ) ) ;
#11062 = FACE_OUTER_BOUND ( 'NONE', #5177, .T. ) ;
#11063 = DIRECTION ( 'NONE',  ( -1.000000000000000000, -0.000000000000000000, -0.000000000000000000 ) ) ;
#11064 = CARTESIAN_POINT ( 'NONE',  ( -1.724194960439331403, 65.52574505033150842, -22.67620946298737294 ) ) ;
#11065 = CARTESIAN_POINT ( 'NONE',  ( -75.96875000204839523, 73.25176868561975141, 18.25176868561974075 ) ) ;
#11066 = VERTEX_POINT ( 'NONE', #823 ) ;
#11067 = CARTESIAN_POINT ( 'NONE',  ( -76.34375000204839523, 55.00000000000000000, -25.81189881249999729 ) ) ;
#11068 = CIRCLE ( 'NONE', #7459, 25.00000000000000355 ) ;
#11069 = ORIENTED_EDGE ( 'NONE', *, *, #8953, .T. ) ;
#11070 = PLANE ( 'NONE',  #7051 ) ;
#11071 = FACE_OUTER_BOUND ( 'NONE', #6503, .T. ) ;
#11072 = CARTESIAN_POINT ( 'NONE',  ( -44.07137245399455594, 63.91548889941181244, -10.85747687929244165 ) ) ;
#11073 = CARTESIAN_POINT ( 'NONE',  ( -76.06250000204842365, 80.81189881250000440, -10.69163855873948954 ) ) ;
#11074 = CARTESIAN_POINT ( 'NONE',  ( 53.00000000000000000, 47.00000000000000711, -6.000000000000000000 ) ) ;
#11075 = LINE ( 'NONE', #2887, #143 ) ;
#11076 = VECTOR ( 'NONE', #9380, 1000.000000000000000 ) ;
#11077 = AXIS2_PLACEMENT_3D ( 'NONE', #6404, #11830, #5499 ) ;
#11078 = EDGE_LOOP ( 'NONE', ( #11666, #9222, #45 ) ) ;
#11079 = CARTESIAN_POINT ( 'NONE',  ( -74.37500000000008527, 30.00000000000013500, 4.592425496802549123E-15 ) ) ;
#11080 = CARTESIAN_POINT ( 'NONE',  ( -71.93750000204838102, 44.30836144126050158, -25.81189881249999374 ) ) ;
#11081 = CARTESIAN_POINT ( 'NONE',  ( -75.00000000000000000, 55.00000000000000000, -25.00000000000000355 ) ) ;
#11082 = CARTESIAN_POINT ( 'NONE',  ( 39.99999999999999289, 55.00000000000000000, 24.99999999999999645 ) ) ;
#11083 = CARTESIAN_POINT ( 'NONE',  ( 17.10991510816216987, 55.91632096216925163, 6.974641958105268991 ) ) ;
#11084 = CARTESIAN_POINT ( 'NONE',  ( -21.35532735205402943, 76.69866270122111018, -3.646780783107293811 ) ) ;
#11085 = CARTESIAN_POINT ( 'NONE',  ( -75.00000000000000000, 55.00000000000000000, 0.000000000000000000 ) ) ;
#11086 = ORIENTED_EDGE ( 'NONE', *, *, #2937, .F. ) ;
#11087 = LINE ( 'NONE', #3078, #894 ) ;
#11088 = CYLINDRICAL_SURFACE ( 'NONE', #572, 1.499999999999999556 ) ;
#11089 = ORIENTED_EDGE ( 'NONE', *, *, #4490, .T. ) ;
#11090 = CARTESIAN_POINT ( 'NONE',  ( -19.88142569839470042, 67.52672413929985851, 16.89011978890229315 ) ) ;
#11091 = VECTOR ( 'NONE', #4822, 1000.000000000000000 ) ;
#11092 = CARTESIAN_POINT ( 'NONE',  ( -76.62500000204839523, 29.18810118750000626, -10.69163855873949309 ) ) ;
#11093 = DIRECTION ( 'NONE',  ( 0.000000000000000000, 1.000000000000000000, 0.000000000000000000 ) ) ;
#11094 = CARTESIAN_POINT ( 'NONE',  ( -18.73741402030934111, 64.90551912913463184, 18.53518525054827393 ) ) ;
#11095 = AXIS2_PLACEMENT_3D ( 'NONE', #7252, #4543, #4431 ) ;
#11096 = FACE_OUTER_BOUND ( 'NONE', #9727, .T. ) ;
#11097 = ORIENTED_EDGE ( 'NONE', *, *, #2480, .F. ) ;
#11098 = CARTESIAN_POINT ( 'NONE',  ( -73.43750000204839523, 44.30836144126049447, -25.81189881249999019 ) ) ;
#11099 = CARTESIAN_POINT ( 'NONE',  ( -80.00000000000000000, 55.00000000000000000, 0.000000000000000000 ) ) ;
#11100 = CARTESIAN_POINT ( 'NONE',  ( -1.855729112296511385, 44.43418165317581980, -18.33336562707187412 ) ) ;
#11101 = ORIENTED_EDGE ( 'NONE', *, *, #8439, .T. ) ;
#11102 = CARTESIAN_POINT ( 'NONE',  ( -48.81096005563045992, 75.47260553545579853, -5.508156592082438685 ) ) ;
#11103 = CONICAL_SURFACE ( 'NONE', #9014, 5.000000000000000888, 1.047197551196596299 ) ;
#11104 = CARTESIAN_POINT ( 'NONE',  ( -48.52239103406665066, 73.33336493528216238, -10.56581381373428208 ) ) ;
#11105 =( LENGTH_UNIT ( ) NAMED_UNIT ( * ) SI_UNIT ( .MILLI., .METRE. ) );
#11106 = DIRECTION ( 'NONE',  ( -1.000000000000000000, -6.033820786006286457E-17, 0.000000000000000000 ) ) ;
#11107 = DIRECTION ( 'NONE',  ( -0.000000000000000000, -0.000000000000000000, -1.000000000000000000 ) ) ;
#11108 = CARTESIAN_POINT ( 'NONE',  ( -71.99927362086853577, 76.65063509461016622, 12.50000000000143352 ) ) ;
#11109 = ORIENTED_EDGE ( 'NONE', *, *, #5660, .F. ) ;
#11110 = CARTESIAN_POINT ( 'NONE',  ( -77.93750000000000000, 72.67766952966368876, 17.67766952966368521 ) ) ;
#11111 = CARTESIAN_POINT ( 'NONE',  ( -53.23625741230951292, 55.01228365700361422, 0.001247673927939117831 ) ) ;
#11112 = CARTESIAN_POINT ( 'NONE',  ( -46.18628267998333570, 59.48674120129327747, -2.212764751379967976 ) ) ;
#11113 = CONICAL_SURFACE ( 'NONE', #8078, 3.000000000000000000, 0.9599310885968912466 ) ;
#11114 = DIRECTION ( 'NONE',  ( 0.000000000000000000, 1.000000000000000000, 0.000000000000000000 ) ) ;
#11115 = PRODUCT_DEFINITION_SHAPE ( 'NONE', 'NONE',  #11856 ) ;
#11116 = CARTESIAN_POINT ( 'NONE',  ( -80.00000000000001421, 50.75735931288069480, -2.742637315201482462 ) ) ;
#11117 = CARTESIAN_POINT ( 'NONE',  ( -55.21148394789464220, 67.02529821378587371, 7.207524229417598072 ) ) ;
#11118 = ORIENTED_EDGE ( 'NONE', *, *, #9371, .F. ) ;
#11119 = DIRECTION ( 'NONE',  ( -1.000000000000000000, -1.776356839400250465E-15, 0.000000000000000000 ) ) ;
#11120 = DIRECTION ( 'NONE',  ( -1.000000000000000000, -0.000000000000000000, -0.000000000000000000 ) ) ;
#11121 = EDGE_CURVE ( 'NONE', #10179, #9462, #4356, .T. ) ;
#11122 = CARTESIAN_POINT ( 'NONE',  ( 53.00000000000000000, 105.0000000000000142, 6.000000000000000000 ) ) ;
#11123 = B_SPLINE_CURVE_WITH_KNOTS ( 'NONE', 3,
 ( #10440, #8841, #620, #7941, #11576, #3377, #7054, #10674, #3616, #1867, #10856, #3441, #7341, #9068, #9182, #5364, #1755, #5534, #792, #970, #1635, #846, #2604, #8172, #11812, #4408, #11633, #8960, #8059, #8, #9904, #7284, #6210, #3559, #7230, #8231, #2662, #6437 ),
 .UNSPECIFIED., .F., .F.,
 ( 4, 2, 2, 2, 2, 2, 2, 2, 2, 2, 2, 2, 2, 2, 2, 2, 2, 2, 4 ),
 ( 0.04856354657319568446, 0.05008122670620035466, 0.05159890683920503179, 0.05235774690570735995, 0.05311658697220968811, 0.05463426710521434443, 0.05615194723821900769, 0.05766962737122366400, 0.05918730750422832032, 0.06070498763723297664, 0.06146382770373530480, 0.06222266777023762602, 0.06374034790324227540, 0.06525802803624693171, 0.06677570816925158803, 0.06829338830225623047, 0.06981106843526088679, 0.07132874856826554311, 0.07284642870127019942 ),
 .UNSPECIFIED. ) ;
#11124 = CARTESIAN_POINT ( 'NONE',  ( -19.44873419826854999, 75.15323065158862903, -14.79757583295479684 ) ) ;
#11125 = CARTESIAN_POINT ( 'NONE',  ( -73.53125000204838102, 55.00000000000000000, -25.81189881249999729 ) ) ;
#11126 = ORIENTED_EDGE ( 'NONE', *, *, #1253, .T. ) ;
#11127 = CARTESIAN_POINT ( 'NONE',  ( -75.96875000409677625, 44.64466094067260826, -24.99999999999998934 ) ) ;
#11128 = EDGE_LOOP ( 'NONE', ( #6307, #2487 ) ) ;
#11129 = DIRECTION ( 'NONE',  ( 0.000000000000000000, 0.000000000000000000, -1.000000000000000000 ) ) ;
#11130 = CARTESIAN_POINT ( 'NONE',  ( -49.92872185120336326, 69.01842773188042202, 1.373364986375345875 ) ) ;
#11131 = ADVANCED_FACE ( 'NONE', ( #6415 ), #9936, .F. ) ;
#11132 = DIRECTION ( 'NONE',  ( -1.000000000000000000, 0.000000000000000000, 0.000000000000000000 ) ) ;
#11133 = CARTESIAN_POINT ( 'NONE',  ( 39.99999999999999289, 55.00000000000000000, -22.00000000000000000 ) ) ;
#11134 = LINE ( 'NONE', #2161, #8006 ) ;
#11135 = EDGE_LOOP ( 'NONE', ( #5663, #1892, #4357, #11152 ) ) ;
#11136 = CARTESIAN_POINT ( 'NONE',  ( -71.84375000409677625, 30.00000000000001421, 10.35533905932739174 ) ) ;
#11137 = DIRECTION ( 'NONE',  ( 0.000000000000000000, 0.000000000000000000, -1.000000000000000000 ) ) ;
#11138 = FACE_BOUND ( 'NONE', #1868, .T. ) ;
#11139 = CARTESIAN_POINT ( 'NONE',  ( -2.915823261801936628, 55.68730727514731171, -7.019035972284535241 ) ) ;
#11140 = CARTESIAN_POINT ( 'NONE',  ( -3.619482055381507024, 65.46993227710001406, 19.34915035418615048 ) ) ;
#11141 = DIRECTION ( 'NONE',  ( -1.000000000000000000, -0.000000000000000000, -0.000000000000000000 ) ) ;
#11142 = ORIENTED_EDGE ( 'NONE', *, *, #5708, .F. ) ;
#11143 = CARTESIAN_POINT ( 'NONE',  ( 0.000000000000000000, 0.000000000000000000, -1.239675197676287643 ) ) ;
#11144 = DIRECTION ( 'NONE',  ( -0.000000000000000000, -0.000000000000000000, 1.000000000000000000 ) ) ;
#11145 = VERTEX_POINT ( 'NONE', #10046 ) ;
#11146 = ADVANCED_FACE ( 'NONE', ( #10890 ), #4495, .T. ) ;
#11147 = CARTESIAN_POINT ( 'NONE',  ( -7.929357056070021947, 64.91238717040420170, -18.54984206437098493 ) ) ;
#11148 = CARTESIAN_POINT ( 'NONE',  ( -76.34375000204839523, 55.00000000000000000, -25.81189881249999729 ) ) ;
#11149 = LINE ( 'NONE', #9488, #1938 ) ;
#11150 = CARTESIAN_POINT ( 'NONE',  ( -68.34104732181950226, 33.99448141944334623, 0.006743540747238889813 ) ) ;
#11151 = CARTESIAN_POINT ( 'NONE',  ( -42.07074724807011989, 61.10209548959944215, -20.11061483308460751 ) ) ;
#11152 = ORIENTED_EDGE ( 'NONE', *, *, #7688, .F. ) ;
#11153 = CIRCLE ( 'NONE', #831, 24.99999999999999645 ) ;
#11154 = DIRECTION ( 'NONE',  ( -0.8660254037844382635, -0.5000000000000005551, 0.000000000000000000 ) ) ;
#11155 = DIRECTION ( 'NONE',  ( 0.8191520442889885789, 0.000000000000000000, 0.5735764363510507113 ) ) ;
#11156 = DIRECTION ( 'NONE',  ( -1.000000000000000000, -0.000000000000000000, -0.000000000000000000 ) ) ;
#11157 = ORIENTED_EDGE ( 'NONE', *, *, #8000, .F. ) ;
#11158 = CARTESIAN_POINT ( 'NONE',  ( -17.67054322722435700, 69.86867477976171870, 14.86928418406260910 ) ) ;
#11159 = CARTESIAN_POINT ( 'NONE',  ( 12.53956257875718805, 53.16901327126123533, 14.01800940675507867 ) ) ;
#11160 = CARTESIAN_POINT ( 'NONE',  ( 0.000000000000000000, -17.00000000000000000, 0.000000000000000000 ) ) ;
#11161 = EDGE_CURVE ( 'NONE', #1442, #8109, #7709, .T. ) ;
#11162 = DIRECTION ( 'NONE',  ( -1.000000000000000000, -0.000000000000000000, -0.000000000000000000 ) ) ;
#11163 = CARTESIAN_POINT ( 'NONE',  ( -3.000000000000000000, 3.673940397442059375E-16, 0.000000000000000000 ) ) ;
#11164 = ORIENTED_EDGE ( 'NONE', *, *, #349, .F. ) ;
#11165 = CARTESIAN_POINT ( 'NONE',  ( -77.56250000000000000, 37.32233047033631124, 17.67766952966369232 ) ) ;
#11166 = DIRECTION ( 'NONE',  ( -1.000000000000000000, -0.000000000000000000, -0.000000000000000000 ) ) ;
#11167 = DIRECTION ( 'NONE',  ( -1.000000000000000000, 0.000000000000000000, 0.000000000000000000 ) ) ;
#11168 = EDGE_CURVE ( 'NONE', #8743, #9107, #5821, .T. ) ;
#11169 = STYLED_ITEM ( 'NONE', ( #4586 ), #2413 ) ;
#11170 = PRESENTATION_STYLE_ASSIGNMENT (( #7662 ) ) ;
#11171 = CARTESIAN_POINT ( 'NONE',  ( -75.03125000409677625, 44.64466094067250168, 24.99999999999987566 ) ) ;
#11172 = CARTESIAN_POINT ( 'NONE',  ( -57.83638956477260251, 62.82127934421545490, 11.69590706508775213 ) ) ;
#11173 = VERTEX_POINT ( 'NONE', #8385 ) ;
#11174 = CARTESIAN_POINT ( 'NONE',  ( 25.00000000000000000, 76.00000000000000000, 0.000000000000000000 ) ) ;
#11175 = DIRECTION ( 'NONE',  ( 0.000000000000000000, 1.000000000000000000, 0.000000000000000000 ) ) ;
#11176 = EDGE_CURVE ( 'NONE', #7332, #6004, #7419, .T. ) ;
#11177 = LINE ( 'NONE', #5876, #4095 ) ;
#11178 = CARTESIAN_POINT ( 'NONE',  ( -3.351853367131006234, 3.838309248099017079, 3.542476846806594127E-15 ) ) ;
#11179 = CARTESIAN_POINT ( 'NONE',  ( -19.18862861118784124, 74.94684730933501271, -15.07442433330465548 ) ) ;
#11180 = CARTESIAN_POINT ( 'NONE',  ( -78.96875000204839523, 80.81189881250000440, -1.580522963032174394E-15 ) ) ;
#11181 = STYLED_ITEM ( 'NONE', ( #4280 ), #6721 ) ;
#11182 = CIRCLE ( 'NONE', #9850, 1.500000000000001332 ) ;
#11183 = EDGE_LOOP ( 'NONE', ( #11236, #1792, #950, #8271 ) ) ;
#11184 = CARTESIAN_POINT ( 'NONE',  ( -71.84375000204838102, 55.00000000000000000, -25.81189881249999729 ) ) ;
#11185 = ORIENTED_EDGE ( 'NONE', *, *, #11054, .F. ) ;
#11186 = CARTESIAN_POINT ( 'NONE',  ( 7.761716740762911293, 67.37671573469675934, -21.72224607068988789 ) ) ;
#11187 = CARTESIAN_POINT ( 'NONE',  ( -40.00186843037597129, 55.00034269701549761, -14.01977987948117921 ) ) ;
#11188 = DIRECTION ( 'NONE',  ( 0.000000000000000000, -0.000000000000000000, 1.000000000000000000 ) ) ;
#11189 =( BOUNDED_CURVE ( )  B_SPLINE_CURVE ( 2, ( #3508, #2735, #3568, #10862, #2672, #3799, #7642, #6631, #5848 ),
 .UNSPECIFIED., .F., .T. ) 
 B_SPLINE_CURVE_WITH_KNOTS ( ( 3, 2, 2, 2, 3 ),
 ( 0.3168733201082642448, 0.3366713418703649596, 0.3564693636324655635, 0.3762673853945661673, 0.3960654071566668821 ),
 .UNSPECIFIED. ) 
 CURVE ( )  GEOMETRIC_REPRESENTATION_ITEM ( )  RATIONAL_B_SPLINE_CURVE ( ( 1.000000000000000000, 0.9238795325112868495, 1.000000000000000000, 0.9238795325112868495, 1.000000000000000000, 0.9238795325112868495, 1.000000000000000000, 0.9238795325112868495, 1.000000000000000000 ) ) 
 REPRESENTATION_ITEM ( '' )  );
#11190 = CARTESIAN_POINT ( 'NONE',  ( 39.99999999999999289, 55.00000000000000000, -24.99999999999999645 ) ) ;
#11191 = DIRECTION ( 'NONE',  ( 0.8191520442889885789, 0.000000000000000000, 0.5735764363510507113 ) ) ;
#11192 = CARTESIAN_POINT ( 'NONE',  ( -80.00000000000002842, 38.02943725152282184, -1.499996628082202133 ) ) ;
#11193 = ADVANCED_FACE ( 'NONE', ( #4792 ), #3195, .F. ) ;
#11194 = ORIENTED_EDGE ( 'NONE', *, *, #3680, .T. ) ;
#11195 = CIRCLE ( 'NONE', #302, 1.500000000000001332 ) ;
#11196 = EDGE_CURVE ( 'NONE', #1807, #9492, #320, .T. ) ;
#11197 = CARTESIAN_POINT ( 'NONE',  ( -74.56250000000008527, 37.32233047033641071, 17.67766952966359639 ) ) ;
#11198 = CARTESIAN_POINT ( 'NONE',  ( -70.93935441986300816, 80.00000000000001421, 6.698726263377743351 ) ) ;
#11199 = CARTESIAN_POINT ( 'NONE',  ( -39.20651884422274946, 51.94919883060119048, -3.974814712047955556 ) ) ;
#11200 = CARTESIAN_POINT ( 'NONE',  ( -78.00000000000001421, 59.24264068711927678, 4.242644059037073312 ) ) ;
#11201 = CARTESIAN_POINT ( 'NONE',  ( 17.89001317236136757, 56.84184411483420263, 6.841298196563591283 ) ) ;
#11202 = CARTESIAN_POINT ( 'NONE',  ( -2.544240217464419196, 65.22984941951537508, 19.47702325593730066 ) ) ;
#11203 = DIRECTION ( 'NONE',  ( -1.000000000000000000, -0.000000000000000000, -0.000000000000000000 ) ) ;
#11204 = EDGE_CURVE ( 'NONE', #11822, #1659, #7555, .T. ) ;
#11205 = ORIENTED_EDGE ( 'NONE', *, *, #445, .T. ) ;
#11206 = DIRECTION ( 'NONE',  ( -1.000000000000000000, -0.000000000000000000, -0.000000000000000000 ) ) ;
#11207 = AXIS2_PLACEMENT_3D ( 'NONE', #11503, #10428, #2292 ) ;
#11208 = CARTESIAN_POINT ( 'NONE',  ( 36.99999999999999289, 55.00000000000000000, -5.249999999999998224 ) ) ;
#11209 = ORIENTED_EDGE ( 'NONE', *, *, #5055, .F. ) ;
#11210 = CARTESIAN_POINT ( 'NONE',  ( -50.85567158358731632, 75.98119253013058483, -2.745941642920928683 ) ) ;
#11211 = CARTESIAN_POINT ( 'NONE',  ( -74.46875000204839523, 80.81189881250000440, -1.580522963032174394E-15 ) ) ;
#11212 = PRODUCT_DEFINITION_SHAPE ( 'NONE', 'NONE',  #1895 ) ;
#11213 = CARTESIAN_POINT ( 'NONE',  ( 5.000000000000000888, 0.000000000000000000, 0.000000000000000000 ) ) ;
#11214 = CARTESIAN_POINT ( 'NONE',  ( -79.90625000000001421, 65.35533905932736332, -24.99999999999996803 ) ) ;
#11215 = VECTOR ( 'NONE', #2035, 1000.000000000000000 ) ;
#11216 = AXIS2_PLACEMENT_3D ( 'NONE', #10353, #10998, #6722 ) ;
#11217 = LINE ( 'NONE', #3027, #2415 ) ;
#11218 = VERTEX_POINT ( 'NONE', #8319 ) ;
#11219 = CYLINDRICAL_SURFACE ( 'NONE', #7231, 1.500000000000000000 ) ;
#11220 = DIRECTION ( 'NONE',  ( -0.000000000000000000, -0.000000000000000000, 1.000000000000000000 ) ) ;
#11221 = CARTESIAN_POINT ( 'NONE',  ( 12.85570563148687739, 52.25434904275299175, 21.01882863504484789 ) ) ;
#11222 = ORIENTED_EDGE ( 'NONE', *, *, #3731, .T. ) ;
#11223 = CARTESIAN_POINT ( 'NONE',  ( 13.52237229673245089, 52.25434890037524127, 21.02046579585209329 ) ) ;
#11224 = AXIS2_PLACEMENT_3D ( 'NONE', #5788, #4821, #313 ) ;
#11225 = CARTESIAN_POINT ( 'NONE',  ( 3.410516172888891084, 41.04393794207129531, -1.373024938261769856 ) ) ;
#11226 = DIRECTION ( 'NONE',  ( -1.000000000000000000, -0.000000000000000000, -0.000000000000000000 ) ) ;
#11227 = SURFACE_STYLE_FILL_AREA ( #10215 ) ;
#11228 = CARTESIAN_POINT ( 'NONE',  ( -78.00000000000000000, 54.99999999999999289, 3.371917797062584654E-06 ) ) ;
#11229 = CARTESIAN_POINT ( 'NONE',  ( -75.68750000409677625, 72.67766952966368876, -17.67766952966368876 ) ) ;
#11230 = VERTEX_POINT ( 'NONE', #10171 ) ;
#11231 = CARTESIAN_POINT ( 'NONE',  ( -76.25000000000000000, 55.00000000000000000, 24.99999999999999645 ) ) ;
#11232 = LINE ( 'NONE', #5926, #8725 ) ;
#11233 = LINE ( 'NONE', #10223, #9965 ) ;
#11234 = FACE_BOUND ( 'NONE', #3704, .T. ) ;
#11235 = CARTESIAN_POINT ( 'NONE',  ( -61.92257069291975569, 53.62718127820116365, 13.95588266757517815 ) ) ;
#11236 = ORIENTED_EDGE ( 'NONE', *, *, #1030, .F. ) ;
#11237 = CARTESIAN_POINT ( 'NONE',  ( 2.500000000000000000, 0.000000000000000000, -2.103846626247716234 ) ) ;
#11238 = CARTESIAN_POINT ( 'NONE',  ( -71.34302368722835297, 77.35376350879521112, 12.90594348738575903 ) ) ;
#11239 = DIRECTION ( 'NONE',  ( -1.000000000000000000, -0.000000000000000000, -0.000000000000000000 ) ) ;
#11240 = CARTESIAN_POINT ( 'NONE',  ( -78.00000000000001421, 67.72792206135787296, 12.72792543327562775 ) ) ;
#11241 = EDGE_CURVE ( 'NONE', #5996, #1761, #5698, .T. ) ;
#11242 = CARTESIAN_POINT ( 'NONE',  ( -25.22862615038675926, 79.94748894109862647, 1.675193470868706180 ) ) ;
#11243 = CARTESIAN_POINT ( 'NONE',  ( -77.56250000204839523, 80.81189881250001861, -10.69163855873949132 ) ) ;
#11244 = ORIENTED_EDGE ( 'NONE', *, *, #2183, .T. ) ;
#11245 = CARTESIAN_POINT ( 'NONE',  ( -78.50000000409677625, 80.00000000000000000, -1.530808498934191324E-15 ) ) ;
#11246 = FACE_BOUND ( 'NONE', #7291, .T. ) ;
#11247 = CARTESIAN_POINT ( 'NONE',  ( 5.000000000000000000, 2.886751345948134428, -0.4465819873852071575 ) ) ;
#11248 = CARTESIAN_POINT ( 'NONE',  ( 18.81101721030213625, 65.56418867429738384, 18.32872549916029925 ) ) ;
#11249 = EDGE_CURVE ( 'NONE', #4880, #9906, #7044, .T. ) ;
#11250 = DIRECTION ( 'NONE',  ( 0.000000000000000000, 1.000000000000000000, 0.000000000000000000 ) ) ;
#11251 =( GEOMETRIC_REPRESENTATION_CONTEXT ( 3 ) GLOBAL_UNCERTAINTY_ASSIGNED_CONTEXT ( ( #5633 ) ) GLOBAL_UNIT_ASSIGNED_CONTEXT ( ( #3108, #7603, #1184 ) ) REPRESENTATION_CONTEXT ( 'NONE', 'WORKASPACE' ) );
#11252 = CARTESIAN_POINT ( 'NONE',  ( -75.00000000000004263, 59.49947659938870714, -25.42130211060962353 ) ) ;
#11253 = CARTESIAN_POINT ( 'NONE',  ( 0.000000000000000000, 0.000000000000000000, -6.099999999999997868 ) ) ;
#11254 = B_SPLINE_CURVE_WITH_KNOTS ( 'NONE', 3,
 ( #26, #5495, #10933, #5620 ),
 .UNSPECIFIED., .F., .F.,
 ( 4, 4 ),
 ( 2.380735200817108042E-07, 0.002921158011986720298 ),
 .UNSPECIFIED. ) ;
#11255 = ORIENTED_EDGE ( 'NONE', *, *, #7278, .T. ) ;
#11256 = CARTESIAN_POINT ( 'NONE',  ( -75.59375000000000000, 44.64466094067260826, -24.99999999999998934 ) ) ;
#11257 = CARTESIAN_POINT ( 'NONE',  ( -74.46875000409679046, 44.64466094067260826, -24.99999999999998934 ) ) ;
#11258 = VECTOR ( 'NONE', #6650, 1000.000000000000000 ) ;
#11259 = CARTESIAN_POINT ( 'NONE',  ( -46.99165357442934976, 58.05298380892439525, -3.973364261919617224 ) ) ;
#11260 = ORIENTED_EDGE ( 'NONE', *, *, #10177, .F. ) ;
#11261 =( BOUNDED_CURVE ( )  B_SPLINE_CURVE ( 2, ( #2123, #5851, #1219, #4886, #4049, #8537, #3986, #7646, #6757 ),
 .UNSPECIFIED., .F., .T. ) 
 B_SPLINE_CURVE_WITH_KNOTS ( ( 3, 2, 2, 2, 3 ),
 ( 0.08333333333333339810, 0.1041666666666667546, 0.1250000000000001110, 0.1458333333333334814, 0.1666666666666667962 ),
 .UNSPECIFIED. ) 
 CURVE ( )  GEOMETRIC_REPRESENTATION_ITEM ( )  RATIONAL_B_SPLINE_CURVE ( ( 0.9999999999999997780, 0.9238795325112869605, 1.000000000000000000, 0.9238795325112867385, 1.000000000000000000, 0.9238795325112867385, 1.000000000000000000, 0.9238795325112861834, 1.000000000000000444 ) ) 
 REPRESENTATION_ITEM ( '' )  );
#11262 = CARTESIAN_POINT ( 'NONE',  ( -7.000135551824203439, 59.95344092836027272, -4.953904230404519105 ) ) ;
#11263 = DIRECTION ( 'NONE',  ( 0.000000000000000000, 1.000000000000000000, 0.000000000000000000 ) ) ;
#11264 = CARTESIAN_POINT ( 'NONE',  ( -78.00000000000002842, 59.24264068711927678, 12.72792543327563131 ) ) ;
#11265 = CIRCLE ( 'NONE', #8221, 3.000000000000000000 ) ;
#11266 = ORIENTED_EDGE ( 'NONE', *, *, #206, .F. ) ;
#11267 = DIRECTION ( 'NONE',  ( -1.000000000000000000, 0.000000000000000000, -0.000000000000000000 ) ) ;
#11268 = CARTESIAN_POINT ( 'NONE',  ( -77.93750000204838102, 65.69163855873948421, -25.81189881250000084 ) ) ;
#11269 = EDGE_LOOP ( 'NONE', ( #7258, #1920 ) ) ;
#11270 = CARTESIAN_POINT ( 'NONE',  ( -26.81096152405270061, 44.41979049410412017, 18.36814973051028588 ) ) ;
#11271 = CARTESIAN_POINT ( 'NONE',  ( -73.06250000204840944, 80.81189881250001861, -10.69163855873949132 ) ) ;
#11272 = EDGE_CURVE ( 'NONE', #8769, #2643, #7607, .T. ) ;
#11273 = CONICAL_SURFACE ( 'NONE', #6138, 5.000000000000000888, 1.047197551196596299 ) ;
#11274 = FACE_OUTER_BOUND ( 'NONE', #6361, .T. ) ;
#11275 = CARTESIAN_POINT ( 'NONE',  ( -59.88037020503378471, 51.91452991566635689, 20.80113349088246011 ) ) ;
#11276 =( LENGTH_UNIT ( ) NAMED_UNIT ( * ) SI_UNIT ( .MILLI., .METRE. ) );
#11277 = FACE_OUTER_BOUND ( 'NONE', #8969, .T. ) ;
#11278 = VERTEX_POINT ( 'NONE', #229 ) ;
#11279 = CARTESIAN_POINT ( 'NONE',  ( -72.12500000204839523, 29.18810118750000626, -10.69163855873949132 ) ) ;
#11280 = EDGE_CURVE ( 'NONE', #932, #4386, #118, .T. ) ;
#11281 = CARTESIAN_POINT ( 'NONE',  ( 0.2637464422577515122, 50.75252801053527207, -2.643076731290110448 ) ) ;
#11282 = VECTOR ( 'NONE', #11312, 1000.000000000000000 ) ;
#11283 = CARTESIAN_POINT ( 'NONE',  ( -10.83980928483403794, 72.54296691076741865, -11.73126556815853760 ) ) ;
#11284 = EDGE_LOOP ( 'NONE', ( #3796, #3729, #575, #8095 ) ) ;
#11285 = CARTESIAN_POINT ( 'NONE',  ( 5.302689875203906666, 34.00688940836099050, 1.031260791178478797 ) ) ;
#11286 = CARTESIAN_POINT ( 'NONE',  ( -54.59603348275399526, 73.54984634329692028, 9.912388241271610667 ) ) ;
#11287 = FACE_OUTER_BOUND ( 'NONE', #8246, .T. ) ;
#11288 = CARTESIAN_POINT ( 'NONE',  ( -77.75000000409677625, 30.00000000000000355, 4.592425496802573578E-15 ) ) ;
#11289 = UNCERTAINTY_MEASURE_WITH_UNIT (LENGTH_MEASURE( 1.000000000000000082E-05 ), #5611, 'distance_accuracy_value', 'NONE');
#11290 = AXIS2_PLACEMENT_3D ( 'NONE', #56, #3724, #1862 ) ;
#11291 = LINE ( 'NONE', #8493, #179 ) ;
#11292 = EDGE_LOOP ( 'NONE', ( #995, #7129 ) ) ;
#11293 = CARTESIAN_POINT ( 'NONE',  ( -77.18750000000000000, 37.32233047033631124, -17.67766952966368166 ) ) ;
#11294 = LINE ( 'NONE', #11585, #5667 ) ;
#11295 = VECTOR ( 'NONE', #227, 1000.000000000000000 ) ;
#11296 = CARTESIAN_POINT ( 'NONE',  ( 14.99999999999999645, -30.00000000000000000, -10.00000000000000000 ) ) ;
#11297 = AXIS2_PLACEMENT_3D ( 'NONE', #2587, #10656, #11496 ) ;
#11298 = AXIS2_PLACEMENT_3D ( 'NONE', #8940, #7037, #6135 ) ;
#11299 = DIRECTION ( 'NONE',  ( -1.000000000000000000, -0.000000000000000000, -0.000000000000000000 ) ) ;
#11300 = CARTESIAN_POINT ( 'NONE',  ( -8.582943931441322505, 58.30613956700960898, -6.186730322951330407 ) ) ;
#11301 = ORIENTED_EDGE ( 'NONE', *, *, #8943, .T. ) ;
#11302 = CARTESIAN_POINT ( 'NONE',  ( -24.81096152833125856, 44.41791055217656492, 18.37268719335390443 ) ) ;
#11303 = DIRECTION ( 'NONE',  ( 0.000000000000000000, 0.000000000000000000, -1.000000000000000000 ) ) ;
#11304 = CARTESIAN_POINT ( 'NONE',  ( 53.00000000000000000, 51.46446609406726935, 3.535533905932731091 ) ) ;
#11305 = CARTESIAN_POINT ( 'NONE',  ( -75.12500000204838102, 29.18810118750000626, -10.69163855873949132 ) ) ;
#11306 = FACE_OUTER_BOUND ( 'NONE', #2371, .T. ) ;
#11307 = CARTESIAN_POINT ( 'NONE',  ( -73.62500000204839523, 44.30836144126050158, -25.81189881249999374 ) ) ;
#11308 = EDGE_LOOP ( 'NONE', ( #10029, #1010, #8391, #6217, #3905, #8088 ) ) ;
#11309 = CARTESIAN_POINT ( 'NONE',  ( -77.09375000409677625, 80.00000000000001421, -10.35533905932737753 ) ) ;
#11310 = AXIS2_PLACEMENT_3D ( 'NONE', #10992, #9930, #11836 ) ;
#11311 = AXIS2_PLACEMENT_3D ( 'NONE', #8954, #7444, #6206 ) ;
#11312 = DIRECTION ( 'NONE',  ( -1.000000000000000000, -0.000000000000000000, -0.000000000000000000 ) ) ;
#11313 = CARTESIAN_POINT ( 'NONE',  ( -53.12201214189175147, 66.25487413167280693, 8.346098093582366317 ) ) ;
#11314 = CLOSED_SHELL ( 'NONE', ( #2940, #9711, #4843, #8700, #5662, #1306, #2097, #1819, #7178, #9306, #9894, #629, #4341, #4111, #10256, #6314, #7712, #5957, #10372 ) ) ;
#11315 = CARTESIAN_POINT ( 'NONE',  ( -78.50000000204842365, 29.18810118750000981, 10.69163855873950020 ) ) ;
#11316 = CARTESIAN_POINT ( 'NONE',  ( -1.734723475976807094E-14, -5.773502691896260863, -5.653418012614792154 ) ) ;
#11317 = FACE_OUTER_BOUND ( 'NONE', #1677, .T. ) ;
#11318 = ORIENTED_EDGE ( 'NONE', *, *, #2521, .F. ) ;
#11319 = CARTESIAN_POINT ( 'NONE',  ( -76.43750000000000000, 72.67766952966368876, 17.67766952966368521 ) ) ;
#11320 = CARTESIAN_POINT ( 'NONE',  ( -70.87427368927673399, 76.65063840437987608, 12.49999426731031527 ) ) ;
#11321 = CARTESIAN_POINT ( 'NONE',  ( -43.87781470623360747, 55.65760560131963786, -4.959288383363730901 ) ) ;
#11322 = ORIENTED_EDGE ( 'NONE', *, *, #8595, .T. ) ;
#11323 = CARTESIAN_POINT ( 'NONE',  ( -10.89008531556037163, 61.97464205804329396, -0.9163204594661494840 ) ) ;
#11324 = DIRECTION ( 'NONE',  ( 0.000000000000000000, 0.000000000000000000, -1.000000000000000000 ) ) ;
#11325 = EDGE_CURVE ( 'NONE', #9242, #541, #1690, .T. ) ;
#11326 = CYLINDRICAL_SURFACE ( 'NONE', #8162, 1.499999999999999556 ) ;
#11327 = ORIENTED_EDGE ( 'NONE', *, *, #9813, .T. ) ;
#11328 = CARTESIAN_POINT ( 'NONE',  ( -74.75000000000000000, 55.00000000000000000, 24.99999999999999645 ) ) ;
#11329 = CARTESIAN_POINT ( 'NONE',  ( -76.62500000204838102, 44.30836144126049447, -25.81189881249999019 ) ) ;
#11330 = EDGE_LOOP ( 'NONE', ( #469, #4971 ) ) ;
#11331 = CARTESIAN_POINT ( 'NONE',  ( -25.18906244525692983, 49.50751464484449826, 20.43480895838654376 ) ) ;
#11332 = LINE ( 'NONE', #2236, #7092 ) ;
#11333 = CARTESIAN_POINT ( 'NONE',  ( -78.87500000409677625, 55.00000000000000000, -24.99999999999999645 ) ) ;
#11334 = CARTESIAN_POINT ( 'NONE',  ( -44.39182476880109363, 68.38060868816502591, -16.29271878486493463 ) ) ;
#11335 =( LENGTH_UNIT ( ) NAMED_UNIT ( * ) SI_UNIT ( .MILLI., .METRE. ) );
#11336 = CARTESIAN_POINT ( 'NONE',  ( 0.000000000000000000, 0.000000000000000000, -2.103846626247716234 ) ) ;
#11337 = VERTEX_POINT ( 'NONE', #10292 ) ;
#11338 = DIRECTION ( 'NONE',  ( -1.000000000000000000, -0.000000000000000000, -0.000000000000000000 ) ) ;
#11339 = ADVANCED_FACE ( 'NONE', ( #164, #1125 ), #4856, .F. ) ;
#11340 = CARTESIAN_POINT ( 'NONE',  ( -0.8192951148925879945, 5.300482436767278926, -0.1983443223721591819 ) ) ;
#11341 = CARTESIAN_POINT ( 'NONE',  ( -8.214759031591983174, 65.81066618478850216, -18.03675305545087681 ) ) ;
#11342 = EDGE_LOOP ( 'NONE', ( #3429, #11583, #11126, #9155 ) ) ;
#11343 = CARTESIAN_POINT ( 'NONE',  ( -67.48465754769044622, 34.52249208990708951, 5.502706378135331811 ) ) ;
#11344 = CARTESIAN_POINT ( 'NONE',  ( -18.16357859702436173, 66.69092602918284740, 7.816436488534476368 ) ) ;
#11345 = DIRECTION ( 'NONE',  ( 1.000000000000000000, 0.000000000000000000, 0.000000000000000000 ) ) ;
#11346 = CARTESIAN_POINT ( 'NONE',  ( -75.96875000409676204, 44.64466094067271484, -25.00000000000010303 ) ) ;
#11347 = DIRECTION ( 'NONE',  ( 0.000000000000000000, -0.000000000000000000, 1.000000000000000000 ) ) ;
#11348 = ADVANCED_FACE ( 'NONE', ( #7612 ), #508, .F. ) ;
#11349 = EDGE_LOOP ( 'NONE', ( #764, #11616, #8823, #3632 ) ) ;
#11350 = CARTESIAN_POINT ( 'NONE',  ( -78.96875000000000000, 30.00000000000001421, 10.35533905932739174 ) ) ;
#11351 = CARTESIAN_POINT ( 'NONE',  ( -74.99999999999997158, 43.66642528933169132, -23.23653603557184155 ) ) ;
#11352 = AXIS2_PLACEMENT_3D ( 'NONE', #5384, #11046, #7483 ) ;
#11353 = FACE_OUTER_BOUND ( 'NONE', #8589, .T. ) ;
#11354 = CARTESIAN_POINT ( 'NONE',  ( -78.00000000000001421, 59.24264068711928388, -14.22791868944003646 ) ) ;
#11355 = CARTESIAN_POINT ( 'NONE',  ( -37.55675198932200232, 49.41446278833375771, -4.289664455798599896 ) ) ;
#11356 = EDGE_LOOP ( 'NONE', ( #11825, #2761, #10949, #3764 ) ) ;
#11357 = EDGE_CURVE ( 'NONE', #1492, #2813, #4011, .T. ) ;
#11358 = CARTESIAN_POINT ( 'NONE',  ( -34.14426257084027583, 36.62727174719971401, -10.58198811264723282 ) ) ;
#11359 = DIRECTION ( 'NONE',  ( 0.000000000000000000, 0.000000000000000000, 1.000000000000000000 ) ) ;
#11360 = LINE ( 'NONE', #4122, #2953 ) ;
#11361 = CARTESIAN_POINT ( 'NONE',  ( -76.81250000204839523, 29.18810118750000981, 10.69163855873950020 ) ) ;
#11362 = CARTESIAN_POINT ( 'NONE',  ( -80.00000000000001421, 67.72792206135787296, -12.72791868944004534 ) ) ;
#11363 = CARTESIAN_POINT ( 'NONE',  ( -73.43750000204839523, 65.69163855873948421, -25.81189881250000440 ) ) ;
#11364 = ORIENTED_EDGE ( 'NONE', *, *, #1668, .T. ) ;
#11365 = CARTESIAN_POINT ( 'NONE',  ( -76.81250000409679046, 72.67766952966368876, 17.67766952966368521 ) ) ;
#11366 = ORIENTED_EDGE ( 'NONE', *, *, #6504, .F. ) ;
#11367 =( LENGTH_UNIT ( ) NAMED_UNIT ( * ) SI_UNIT ( .MILLI., .METRE. ) );
#11368 = CARTESIAN_POINT ( 'NONE',  ( -16.69731055678936826, 70.57278980777935828, 14.11442052818484783 ) ) ;
#11369 = DIRECTION ( 'NONE',  ( -1.000000000000000000, -0.000000000000000000, -0.000000000000000000 ) ) ;
#11370 = CARTESIAN_POINT ( 'NONE',  ( -78.00000000000001421, 67.72792206135787296, 11.22792543327562775 ) ) ;
#11371 = DIRECTION ( 'NONE',  ( 0.000000000000000000, 0.000000000000000000, -1.000000000000000000 ) ) ;
#11372 =( GEOMETRIC_REPRESENTATION_CONTEXT ( 3 ) GLOBAL_UNCERTAINTY_ASSIGNED_CONTEXT ( ( #9333 ) ) GLOBAL_UNIT_ASSIGNED_CONTEXT ( ( #2744, #7248, #10153 ) ) REPRESENTATION_CONTEXT ( 'NONE', 'WORKASPACE' ) );
#11373 = VERTEX_POINT ( 'NONE', #6478 ) ;
#11374 = CARTESIAN_POINT ( 'NONE',  ( -78.12500000000000000, 80.00000000000000000, -1.530808498934191324E-15 ) ) ;
#11375 = CARTESIAN_POINT ( 'NONE',  ( 36.99999999999999289, 50.00000000000001421, 6.123233995736750505E-16 ) ) ;
#11376 = DIRECTION ( 'NONE',  ( -1.000000000000000000, -0.000000000000000000, -0.000000000000000000 ) ) ;
#11377 = ORIENTED_EDGE ( 'NONE', *, *, #10548, .F. ) ;
#11378 = CARTESIAN_POINT ( 'NONE',  ( -40.54150824691468102, 56.02863368430912772, -6.936948454549333398 ) ) ;
#11379 = PRODUCT_DEFINITION_FORMATION_WITH_SPECIFIED_SOURCE ( 'ANY', '', #7768, .NOT_KNOWN. ) ;
#11380 = CARTESIAN_POINT ( 'NONE',  ( -73.25000000000000000, 55.00000000000000000, 24.99999999999999645 ) ) ;
#11381 = CARTESIAN_POINT ( 'NONE',  ( -80.00000000000002842, 54.99999999999998579, 9.985284746156354529 ) ) ;
#11382 = B_SPLINE_SURFACE_WITH_KNOTS ( 'NONE', 3, 3, ( 
 ( #617, #8891, #8836, #672, #4343, #3258, #4279, #1578, #3373, #3498, #11448, #3435, #11630, #10733, #497, #729, #6930, #10560, #10789, #10609, #5182, #7108, #2418, #9781, #7049, #6089, #2360, #9612, #2541, #7164, #1404, #6207, #10671, #4219, #5069, #8775, #3320, #7993, #9721, #9841, #1632, #6147, #8714, #7881, #8054, #11697, #5244, #4156, #7817, #6031, #11512, #9666, #1464, #5126, #5300, #553, #1518, #7938, #2482, #11016, #4462, #9118, #3, #2659, #1753, #1695, #3555, #5359, #4631, #9237, #9899, #10911, #8114, #1025, #901, #2720, #6495, #1926, #6381, #9065, #842, #2773, #10852, #3673, #11749, #4573, #6267, #10009, #7225, #5471, #788, #966, #6326, #59, #8282, #9956, #8227, #3725, #5417, #6433, #9010, #4513, #3787, #121, #7389, #10065, #9178, #4685, #8168, #7336, #2599, #2828, #10962, #8337, #11809, #10124, #7456, #3613, #1864, #7280, #1803, #5599, #5530, #5720 ),
 ( #10426, #7631, #2167, #2955, #8590, #10310, #9290, #11201, #11083, #9355, #7689, #4087, #6619, #5897, #4874, #9417, #2894, #2228, #2045, #4995, #186, #9540, #366, #1331, #4751, #6742, #6563, #3972, #1144, #10193, #3073, #11139, #2106, #4031, #1266, #1086, #5781, #4935, #8403, #11262, #1985, #3853, #428, #8647, #11323, #10373, #5837, #5653, #7518, #1208, #10248, #3132, #8524, #4814, #8469, #6799, #246, #3910, #9477, #7574, #3011, #6680, #308, #2350, #6019, #9601, #3360, #1508, #7096, #4269, #10658, #11438, #5233, #6975, #5962, #7868, #7747, #9654, #4325, #717, #3247, #2531, #5170, #6078, #11378, #10719, #10547, #1620, #8703, #6197, #8881, #9831, #1394, #7036, #3188, #606, #1449, #6861, #11557, #7806, #10600, #5114, #10485, #8762, #543, #2468, #4207, #6134, #1568, #7926, #2289, #11500, #5285, #8939, #9769, #5056, #486, #4143, #3308, #6916, #2404, #9712, #659, #8824 ),
 ( #7982, #11619, #3422, #7327, #775, #3716, #10777, #7214, #9054, #7154, #9226, #11680, #6424, #5406, #4389, #1853, #2590, #3540, #10839, #9000, #1794, #3489, #4503, #4618, #6373, #7379, #8156, #2709, #9999, #9945, #8104, #890, #11850, #6256, #9884, #5520, #4564, #830, #3603, #11006, #11798, #2819, #6486, #5461, #1679, #7268, #5348, #2645, #6311, #10054, #8273, #2763, #10115, #9109, #8216, #1913, #5583, #3663, #10953, #4451, #8042, #11740, #1742, #10898, #9167, #952, #47, #3061, #2031, #5883, #10362, #3777, #173, #3841, #5643, #10299, #108, #1133, #1252, #3000, #4020, #4800, #11187, #6670, #6610, #4739, #9405, #8327, #1013, #7445, #11072, #7677, #2883, #8458, #7508, #11130, #5707, #4922, #6730, #4674, #5828, #11313, #6550, #295, #2157, #237, #10181, #2095, #8575, #353, #2217, #1974, #9467, #3122, #5767, #9279, #1071, #8393, #7563, #2943, #6787, #10416, #1199, #3958 ),
 ( #3900, #8513, #4864, #10237, #9344, #7620, #11248, #2454, #4078, #647, #6848, #10472, #2518, #2339, #8747, #10640, #10531, #1497, #6963, #6008, #2272, #9527, #6119, #10705, #7080, #9754, #10588, #9641, #4131, #1315, #4309, #7967, #5948, #531, #4984, #3346, #2389, #3408, #473, #7018, #8634, #11602, #8811, #7793, #1437, #1551, #7854, #11426, #3233, #11368, #5156, #3294, #8867, #6065, #588, #1384, #5218, #4194, #7737, #5102, #415, #6903, #3177, #9586, #5045, #8691, #9699, #11482, #4254, #7913, #11542, #203, #7140, #9311, #7475, #5670, #11665, #1943, #1606, #11034, #8091, #5273, #10141, #6240, #5548, #4434, #11151, #8983, #3525, #1039, #2629, #9250, #137, #6513, #6182, #11726, #1100, #4763, #5612, #9814, #8921, #8419, #7196, #3870, #702, #4375, #4705, #7529, #8026, #3475, #1999, #2911, #10762, #984, #3741, #9869, #5332, #2573, #1663, #759, #8357, #10821, #6450, #10081 ) ),
 .UNSPECIFIED., .F., .F., .F.,
 ( 4, 4 ),
 ( 4, 2, 2, 2, 2, 2, 2, 2, 2, 2, 2, 2, 2, 2, 2, 2, 2, 2, 2, 2, 2, 2, 2, 2, 2, 2, 2, 2, 2, 2, 2, 2, 2, 2, 2, 2, 2, 2, 2, 2, 2, 2, 2, 2, 2, 2, 2, 2, 2, 2, 2, 2, 2, 2, 2, 2, 2, 2, 2, 2, 2, 4 ),
 ( 0.000000000000000000, 1.000000000000000000 ),
 ( 0.000000000000000000, 0.02499977550252127645, 0.04999988577693819519, 0.07499999605135511394, 0.09999999831535408279, 0.1250000005793530378, 0.1500000028441162425, 0.1750000051088794195, 0.1937500039558066045, 0.2031250033792701970, 0.2125000028027338173, 0.2218750022261974375, 0.2312500016496610300, 0.2500000004965882150, 0.2750000027613288545, 0.3000000050260694384, 0.3187500038730080032, 0.3281250032964772578, 0.3375000027199465125, 0.3468750021434158226, 0.3562500015668850772, 0.3750000004138236420, 0.4000000026785641705, 0.4250000049433046989, 0.4437500037902432082, 0.4531250032137125183, 0.4625000026371817730, 0.4718750020606510276, 0.4812500014841203377, 0.5000000003310588470, 0.5250000025957997085, 0.5500000048605405700, 0.5687500037074788573, 0.5781250031309480564, 0.5875000025544172555, 0.5968750019778864546, 0.6062500014013556537, 0.6250000002482940520, 0.6500000025128280789, 0.6750000047773621059, 0.6937500036244039769, 0.7031250030479249125, 0.7125000024714458480, 0.7218750018949667835, 0.7312500013184877190, 0.7500000001655295900, 0.7750000023794885173, 0.8000000045934475557, 0.8187500034657768655, 0.8281250029019414649, 0.8375000023381060643, 0.8468750017742707747, 0.8562500012104353742, 0.8750000000827646840, 0.8937502654913498379, 0.9031253981956424148, 0.9125005308999349918, 0.9218756636042275687, 0.9312507963085201457, 0.9500010617171052996, 0.9750005308585526498, 1.000000000000000000 ),
 .UNSPECIFIED. ) ;
#11383 = ORIENTED_EDGE ( 'NONE', *, *, #2510, .T. ) ;
#11384 = CARTESIAN_POINT ( 'NONE',  ( 18.41262152147913156, 74.28295599064558985, 10.66131699734120275 ) ) ;
#11385 = DIRECTION ( 'NONE',  ( -1.000000000000000000, 0.000000000000000000, 0.000000000000000000 ) ) ;
#11386 = ORIENTED_EDGE ( 'NONE', *, *, #6255, .T. ) ;
#11387 = CARTESIAN_POINT ( 'NONE',  ( -74.84375000204839523, 55.00000000000000000, -25.81189881249999729 ) ) ;
#11388 = DIRECTION ( 'NONE',  ( -1.000000000000000000, -0.000000000000000000, -0.000000000000000000 ) ) ;
#11389 = CARTESIAN_POINT ( 'NONE',  ( 0.000000000000000000, 0.000000000000000000, -6.099999999999999645 ) ) ;
#11390 = ORIENTED_EDGE ( 'NONE', *, *, #7782, .T. ) ;
#11391 = DIRECTION ( 'NONE',  ( -1.000000000000000000, 0.000000000000000000, -0.000000000000000000 ) ) ;
#11392 = ADVANCED_FACE ( 'NONE', ( #10105 ), #1905, .F. ) ;
#11393 = CARTESIAN_POINT ( 'NONE',  ( -34.72515708538001888, 34.82355399787605421, -6.128525890628534256 ) ) ;
#11394 = EDGE_LOOP ( 'NONE', ( #8332, #3521, #9807 ) ) ;
#11395 = CARTESIAN_POINT ( 'NONE',  ( -63.73338128346249221, 41.62050876239434416, 16.30218879057518322 ) ) ;
#11396 = CARTESIAN_POINT ( 'NONE',  ( -31.87813363146436885, 41.40035587688806373, 3.406667234184215243 ) ) ;
#11397 = CARTESIAN_POINT ( 'NONE',  ( 39.99999999999999289, 55.00000000000000000, 22.00000000000000000 ) ) ;
#11398 = CARTESIAN_POINT ( 'NONE',  ( 0.000000000000000000, 5.773502691896260863, -0.4465819873852071575 ) ) ;
#11399 = CARTESIAN_POINT ( 'NONE',  ( -17.81440531450395071, 59.49424450570884204, 2.215684812588340158 ) ) ;
#11400 = VECTOR ( 'NONE', #2001, 1000.000000000000000 ) ;
#11401 = ORIENTED_EDGE ( 'NONE', *, *, #4460, .F. ) ;
#11402 = CARTESIAN_POINT ( 'NONE',  ( -79.34375000204839523, 73.25176868561975141, -18.25176868561974430 ) ) ;
#11403 = CARTESIAN_POINT ( 'NONE',  ( -74.99999999999998579, 45.21990583575040290, -23.90237970175139637 ) ) ;
#11404 = EDGE_CURVE ( 'NONE', #5117, #2595, #1802, .T. ) ;
#11405 = SURFACE_SIDE_STYLE ('',( #5141 ) ) ;
#11406 = EDGE_CURVE ( 'NONE', #546, #1153, #706, .T. ) ;
#11407 = EDGE_CURVE ( 'NONE', #818, #8743, #8560, .T. ) ;
#11408 = CIRCLE ( 'NONE', #6090, 3.000000000000002665 ) ;
#11409 = DIRECTION ( 'NONE',  ( -1.000000000000000000, -0.000000000000000000, -0.000000000000000000 ) ) ;
#11410 = CARTESIAN_POINT ( 'NONE',  ( -18.50022343123301027, 60.84416894878899740, 3.906748298023257071 ) ) ;
#11411 = VERTEX_POINT ( 'NONE', #7477 ) ;
#11412 = CARTESIAN_POINT ( 'NONE',  ( -19.32947785509334082, 63.04547287423799418, 19.42212676744230393 ) ) ;
#11413 = CARTESIAN_POINT ( 'NONE',  ( 22.18771278451687579, 76.01886845420673922, 2.750080521686579793 ) ) ;
#11414 = DIRECTION ( 'NONE',  ( -0.000000000000000000, 0.000000000000000000, 1.000000000000000000 ) ) ;
#11415 = CARTESIAN_POINT ( 'NONE',  ( -75.50000000204840944, 44.30836144126052289, 25.81189881250000795 ) ) ;
#11416 = CARTESIAN_POINT ( 'NONE',  ( -8.150614517903754574, 67.55343220693646344, 21.62334187180388767 ) ) ;
#11417 = CARTESIAN_POINT ( 'NONE',  ( -76.53125000204839523, 36.74823131438024859, -18.25176868561973720 ) ) ;
#11418 = EDGE_CURVE ( 'NONE', #8673, #8424, #139, .T. ) ;
#11419 = ADVANCED_FACE ( 'NONE', ( #1221 ), #5672, .T. ) ;
#11420 = VERTEX_POINT ( 'NONE', #3872 ) ;
#11421 = CARTESIAN_POINT ( 'NONE',  ( -73.53125000409676204, 44.64466094067262958, 25.00000000000001066 ) ) ;
#11422 = FACE_BOUND ( 'NONE', #8553, .T. ) ;
#11423 = CARTESIAN_POINT ( 'NONE',  ( 52.99999999999999289, 58.53553390593273065, 3.535533905932731091 ) ) ;
#11424 = CIRCLE ( 'NONE', #6100, 3.000000000000000888 ) ;
#11425 = EDGE_CURVE ( 'NONE', #3357, #4223, #5311, .T. ) ;
#11426 = CARTESIAN_POINT ( 'NONE',  ( -15.27494751580540111, 73.62981360231496808, 9.945832149094092856 ) ) ;
#11427 = DIRECTION ( 'NONE',  ( 1.000000000000000000, 6.033820786006286457E-17, -0.000000000000000000 ) ) ;
#11428 =( REPRESENTATION_RELATIONSHIP ('NONE','NONE', #5489, #4172 ) REPRESENTATION_RELATIONSHIP_WITH_TRANSFORMATION ( #1804 )SHAPE_REPRESENTATION_RELATIONSHIP( ) );
#11429 = PLANE ( 'NONE',  #4148 ) ;
#11430 = CARTESIAN_POINT ( 'NONE',  ( 3.000000000000000000, 3.673940397442059868E-16, -5.210428571428570521 ) ) ;
#11431 = VECTOR ( 'NONE', #1964, 1000.000000000000000 ) ;
#11432 = ORIENTED_EDGE ( 'NONE', *, *, #878, .T. ) ;
#11433 = DIRECTION ( 'NONE',  ( -1.000000000000000000, -0.000000000000000000, -0.000000000000000000 ) ) ;
#11434 = CARTESIAN_POINT ( 'NONE',  ( -73.71875000000000000, 80.00000000000001421, -10.35533905932737753 ) ) ;
#11435 = FACE_OUTER_BOUND ( 'NONE', #4718, .T. ) ;
#11436 = DIRECTION ( 'NONE',  ( 0.000000000000000000, 0.000000000000000000, 1.000000000000000000 ) ) ;
#11437 = ORIENTED_EDGE ( 'NONE', *, *, #7825, .F. ) ;
#11438 = CARTESIAN_POINT ( 'NONE',  ( -30.33346888516166118, 47.99444905479163737, 0.0003276040068861179808 ) ) ;
#11439 = DIRECTION ( 'NONE',  ( 0.000000000000000000, 0.000000000000000000, 1.000000000000000000 ) ) ;
#11440 = LINE ( 'NONE', #3249, #1653 ) ;
#11441 = EDGE_LOOP ( 'NONE', ( #5568, #4758 ) ) ;
#11442 = CARTESIAN_POINT ( 'NONE',  ( 5.010510290115603560, 65.89460049710385192, -19.11356980082808832 ) ) ;
#11443 = CARTESIAN_POINT ( 'NONE',  ( -79.43750000204838102, 65.69163855873948421, -25.81189881250000084 ) ) ;
#11444 = ORIENTED_EDGE ( 'NONE', *, *, #10549, .F. ) ;
#11445 = CARTESIAN_POINT ( 'NONE',  ( -74.56250000204839523, 80.81189881250001861, -10.69163855873949132 ) ) ;
#11446 = DIRECTION ( 'NONE',  ( 0.000000000000000000, 0.000000000000000000, 1.000000000000000000 ) ) ;
#11447 = CARTESIAN_POINT ( 'NONE',  ( -78.00000000000000000, 54.99999999999999289, 3.371917797062584654E-06 ) ) ;
#11448 = CARTESIAN_POINT ( 'NONE',  ( 15.09270675947632689, 55.01153773592707097, -0.02355180096384254518 ) ) ;
#11449 = AXIS2_PLACEMENT_3D ( 'NONE', #10411, #2209, #2265 ) ;
#11450 = DIRECTION ( 'NONE',  ( 0.000000000000000000, 0.000000000000000000, 1.000000000000000000 ) ) ;
#11451 = AXIS2_PLACEMENT_3D ( 'NONE', #9751, #4432, #4372 ) ;
#11452 = CARTESIAN_POINT ( 'NONE',  ( -75.00000000000000000, 38.26481293166236242, 18.71712631840276941 ) ) ;
#11453 = ORIENTED_EDGE ( 'NONE', *, *, #8075, .T. ) ;
#11454 = DIRECTION ( 'NONE',  ( 0.000000000000000000, 1.000000000000000000, 0.000000000000000000 ) ) ;
#11455 = ADVANCED_FACE ( 'NONE', ( #1163 ), #3969, .T. ) ;
#11456 = CARTESIAN_POINT ( 'NONE',  ( -47.81092963715463640, 71.80394787507084686, -12.92116392654651058 ) ) ;
#11457 = ORIENTED_EDGE ( 'NONE', *, *, #4529, .T. ) ;
#11458 = CARTESIAN_POINT ( 'NONE',  ( 8.855705142202525693, 38.19481665208223120, 12.92224424505011271 ) ) ;
#11459 = CARTESIAN_POINT ( 'NONE',  ( -4.539499248000766762, 53.16883361098971505, -13.98200185442132160 ) ) ;
#11460 = DIRECTION ( 'NONE',  ( -1.000000000000000000, -0.000000000000000000, -0.000000000000000000 ) ) ;
#11461 =( NAMED_UNIT ( * ) SI_UNIT ( $, .STERADIAN. ) SOLID_ANGLE_UNIT ( ) );
#11462 = CARTESIAN_POINT ( 'NONE',  ( -21.71149157619788994, 57.21358471493454090, 4.495333134771674288 ) ) ;
#11463 = ORIENTED_EDGE ( 'NONE', *, *, #3751, .F. ) ;
#11464 = CARTESIAN_POINT ( 'NONE',  ( -72.06435441788588037, 80.00000000000001421, 6.698726029249594482 ) ) ;
#11465 = CARTESIAN_POINT ( 'NONE',  ( -3.000000000000000000, 0.000000000000000000, -2.617914285714285416 ) ) ;
#11466 = FILL_AREA_STYLE_COLOUR ( '', #3421 ) ;
#11467 = DIRECTION ( 'NONE',  ( -1.000000000000000000, -0.000000000000000000, -0.000000000000000000 ) ) ;
#11468 = CARTESIAN_POINT ( 'NONE',  ( -52.91582296080724035, 62.01289876477373042, 0.6873062178531880173 ) ) ;
#11469 = ORIENTED_EDGE ( 'NONE', *, *, #4890, .T. ) ;
#11470 = CARTESIAN_POINT ( 'NONE',  ( -56.05785376386896246, 64.93131079446247611, 18.59685268580366468 ) ) ;
#11471 = AXIS2_PLACEMENT_3D ( 'NONE', #7879, #184, #9235 ) ;
#11472 = CARTESIAN_POINT ( 'NONE',  ( 7.477680471578420196, 36.66673471410030061, 10.56605622896702990 ) ) ;
#11473 = CYLINDRICAL_SURFACE ( 'NONE', #9070, 1.500000000000000000 ) ;
#11474 = CARTESIAN_POINT ( 'NONE',  ( -74.18750000204839523, 65.69163855873949842, 25.81189881250000084 ) ) ;
#11475 = CARTESIAN_POINT ( 'NONE',  ( -23.80750660682828013, 78.73676915960464839, -7.856738918655103987 ) ) ;
#11476 = CARTESIAN_POINT ( 'NONE',  ( -73.43750000204839523, 44.30836144126050158, -25.81189881249999374 ) ) ;
#11477 = AXIS2_PLACEMENT_3D ( 'NONE', #1786, #5511, #7260 ) ;
#11478 = EDGE_LOOP ( 'NONE', ( #10012, #1090, #1523, #6262 ) ) ;
#11479 = CARTESIAN_POINT ( 'NONE',  ( -72.12500000409677625, 55.00000000000000000, 24.99999999999999645 ) ) ;
#11480 = FACE_BOUND ( 'NONE', #9383, .T. ) ;
#11481 = VERTEX_POINT ( 'NONE', #7707 ) ;
#11482 = CARTESIAN_POINT ( 'NONE',  ( -29.26269115883859939, 34.87241548204915631, 6.108265559058850158 ) ) ;
#11483 = VECTOR ( 'NONE', #8997, 1000.000000000000000 ) ;
#11484 = CIRCLE ( 'NONE', #6347, 25.00000000000000355 ) ;
#11485 = CARTESIAN_POINT ( 'NONE',  ( -76.34375000204839523, 73.25176868561975141, -18.25176868561974430 ) ) ;
#11486 = CARTESIAN_POINT ( 'NONE',  ( 47.00000000000000000, 47.00000000000000711, -6.000000000000000000 ) ) ;
#11487 = ADVANCED_FACE ( 'NONE', ( #9370 ), #11219, .F. ) ;
#11488 = B_SPLINE_CURVE_WITH_KNOTS ( 'NONE', 3,
 ( #3260, #10735, #8957, #10672, #11452, #1579, #3500, #7166, #790, #10561, #4406, #1633, #4345, #8776, #5129, #2361, #9785, #11514, #9902, #730, #5246, #7997, #2486, #2543, #3439, #1697, #8893, #6033, #9668, #10791, #1466, #11631, #674, #618, #557, #4221 ),
 .UNSPECIFIED., .F., .F.,
 ( 4, 2, 2, 2, 2, 2, 2, 2, 2, 2, 2, 2, 2, 2, 2, 2, 2, 4 ),
 ( 2.099783704812584100E-15, 0.003153077943881680070, 0.006306155887761260258, 0.009459233831640840445, 0.01103577280358064051, 0.01261231177552044232, 0.01576538971940004766, 0.01734192869133985293, 0.01891846766327966167, 0.02522462355103887582, 0.02837770149491848290, 0.03153077943879808998, 0.03468385738267770052, 0.03626039635461750926, 0.03783693532655729719, 0.04414309121431648358, 0.04729616915819608719, 0.05044924710207567692 ),
 .UNSPECIFIED. ) ;
#11489 = DIRECTION ( 'NONE',  ( -1.000000000000000000, -0.000000000000000000, -0.000000000000000000 ) ) ;
#11490 = EDGE_LOOP ( 'NONE', ( #5354, #7569, #6998, #947 ) ) ;
#11491 = CARTESIAN_POINT ( 'NONE',  ( 2.500000000000005773, 4.330127018922190985, -6.099999999999999645 ) ) ;
#11492 = CARTESIAN_POINT ( 'NONE',  ( -77.37500000000000000, 30.00000000000000355, 4.592425496802573578E-15 ) ) ;
#11493 = VECTOR ( 'NONE', #1036, 1000.000000000000000 ) ;
#11494 = DIRECTION ( 'NONE',  ( 0.000000000000000000, 0.000000000000000000, 1.000000000000000000 ) ) ;
#11495 = ORIENTED_EDGE ( 'NONE', *, *, #1903, .T. ) ;
#11496 = DIRECTION ( 'NONE',  ( 0.000000000000000000, 0.000000000000000000, 1.000000000000000000 ) ) ;
#11497 = CLOSED_SHELL ( 'NONE', ( #6966, #7106, #9280, #8592, #7195, #512, #4419, #3040, #11574, #4833, #2424, #1698, #11487, #6395, #8853, #6571, #803, #10176, #5080, #3795, #8580, #4676, #9450, #2857, #5015, #7314, #5140, #8288, #6028, #10683, #10247, #5432, #61, #263, #8330, #7507, #6001, #5426, #6470, #7935, #10910, #1592, #5745, #6440, #2734, #5528, #7421, #5545, #660, #11499, #10156, #9127, #6979, #10462, #957, #10400, #11562, #2397, #6224, #1914, #785, #5508 ) ) ;
#11498 = VERTEX_POINT ( 'NONE', #3988 ) ;
#11499 = ADVANCED_FACE ( 'NONE', ( #4832 ), #7589, .F. ) ;
#11500 = CARTESIAN_POINT ( 'NONE',  ( -58.91624683120330275, 54.31316703610227847, 6.983828696265685920 ) ) ;
#11501 = APPLICATION_CONTEXT ( 'automotive_design' ) ;
#11502 = CARTESIAN_POINT ( 'NONE',  ( -77.56250000000007105, 37.32233047033638229, 17.67766952966362837 ) ) ;
#11503 = CARTESIAN_POINT ( 'NONE',  ( 0.000000000000000000, 0.000000000000000000, -6.099999999999999645 ) ) ;
#11504 = VECTOR ( 'NONE', #11692, 1000.000000000000000 ) ;
#11505 = CARTESIAN_POINT ( 'NONE',  ( 3.626376041244185000, 65.46044694857717161, 19.35555878592614931 ) ) ;
#11506 = CARTESIAN_POINT ( 'NONE',  ( -78.31250000204838102, 29.18810118750000626, -10.69163855873949132 ) ) ;
#11507 = EDGE_LOOP ( 'NONE', ( #4680, #3601, #4873, #4370 ) ) ;
#11508 =( BOUNDED_CURVE ( )  B_SPLINE_CURVE ( 2, ( #10993, #11171, #2986, #8313, #6652, #11838, #3648, #7315, #11057 ),
 .UNSPECIFIED., .F., .T. ) 
 B_SPLINE_CURVE_WITH_KNOTS ( ( 3, 2, 2, 2, 3 ),
 ( 0.4166666666666670182, 0.4375000000000003331, 0.4583333333333337034, 0.4791666666666670737, 0.5000000000000004441 ),
 .UNSPECIFIED. ) 
 CURVE ( )  GEOMETRIC_REPRESENTATION_ITEM ( )  RATIONAL_B_SPLINE_CURVE ( ( 0.9999999999999987788, 0.9238795325112879597, 1.000000000000000000, 0.9238795325112867385, 1.000000000000000000, 0.9238795325112867385, 1.000000000000000000, 0.9238795325112850731, 1.000000000000001554 ) ) 
 REPRESENTATION_ITEM ( '' )  );
#11509 = CARTESIAN_POINT ( 'NONE',  ( -77.46875000204839523, 80.81189881250000440, -1.580522963032174394E-15 ) ) ;
#11510 = CARTESIAN_POINT ( 'NONE',  ( 0.000000000000000000, 0.000000000000000000, -0.8895714285714284575 ) ) ;
#11511 = CARTESIAN_POINT ( 'NONE',  ( 52.99999999999999289, 97.00000000000000000, -9.797174393178809880E-16 ) ) ;
#11512 = CARTESIAN_POINT ( 'NONE',  ( -15.99785213383137616, 55.00209440256361404, 0.002335802559052338814 ) ) ;
#11513 =( LENGTH_UNIT ( ) NAMED_UNIT ( * ) SI_UNIT ( .MILLI., .METRE. ) );
#11514 = CARTESIAN_POINT ( 'NONE',  ( -75.00000000000002842, 30.18774035812622714, 5.570907983300552146 ) ) ;
#11515 = ORIENTED_EDGE ( 'NONE', *, *, #10885, .F. ) ;
#11516 = CARTESIAN_POINT ( 'NONE',  ( -2.925285743277529438, -4.084588180558409221, -0.01055556052339341917 ) ) ;
#11517 = EDGE_CURVE ( 'NONE', #9873, #43, #2042, .T. ) ;
#11518 = CARTESIAN_POINT ( 'NONE',  ( -52.27495405780593529, 76.01412898031726684, 2.059423305703688811 ) ) ;
#11519 = VERTEX_POINT ( 'NONE', #1409 ) ;
#11520 = CARTESIAN_POINT ( 'NONE',  ( -49.47762672124542149, 75.47109300164294154, -5.507530253420135580 ) ) ;
#11521 = CARTESIAN_POINT ( 'NONE',  ( -9.121973149755229215, 63.34697924335122821, -11.25570253714172608 ) ) ;
#11522 = CARTESIAN_POINT ( 'NONE',  ( -78.50000000204840944, 29.18810118750000981, 10.69163855873950020 ) ) ;
#11523 = VERTEX_POINT ( 'NONE', #8778 ) ;
#11524 = CARTESIAN_POINT ( 'NONE',  ( -78.03125000204838102, 55.00000000000000000, -25.81189881249999729 ) ) ;
#11525 = CARTESIAN_POINT ( 'NONE',  ( 10.18903847268274276, 38.19250115101311849, 12.92455934260550521 ) ) ;
#11526 = VERTEX_POINT ( 'NONE', #8664 ) ;
#11527 = CARTESIAN_POINT ( 'NONE',  ( 39.99999999999999289, 55.00000000000000000, 0.000000000000000000 ) ) ;
#11528 = CARTESIAN_POINT ( 'NONE',  ( -80.00000000000001421, 63.48528137423857487, -1.499996628082204797 ) ) ;
#11529 = CARTESIAN_POINT ( 'NONE',  ( -45.62461256353399364, 57.99907488884235818, -6.340528469342151752 ) ) ;
#11530 = ORIENTED_EDGE ( 'NONE', *, *, #11418, .F. ) ;
#11531 = CARTESIAN_POINT ( 'NONE',  ( -10.81092923698156838, 75.47407628921179423, -5.508885182882011122 ) ) ;
#11532 = ADVANCED_FACE ( 'NONE', ( #3146 ), #6093, .F. ) ;
#11533 = DIRECTION ( 'NONE',  ( -1.000000000000000000, -0.000000000000000000, -0.000000000000000000 ) ) ;
#11534 = CARTESIAN_POINT ( 'NONE',  ( 2.500000000000003109, -4.330127018922193649, 0.000000000000000000 ) ) ;
#11535 = CARTESIAN_POINT ( 'NONE',  ( -75.68750000204839523, 65.69163855873949842, 25.81189881250000084 ) ) ;
#11536 = CARTESIAN_POINT ( 'NONE',  ( -75.78125000000005684, 30.00000000000011013, -10.35533905932734022 ) ) ;
#11537 = CARTESIAN_POINT ( 'NONE',  ( -72.21875000204838102, 29.18810118750000271, 4.741568889096522788E-15 ) ) ;
#11538 = ORIENTED_EDGE ( 'NONE', *, *, #3317, .F. ) ;
#11539 = CARTESIAN_POINT ( 'NONE',  ( -74.18750000409677625, 72.67766952966368876, -17.67766952966368876 ) ) ;
#11540 = CYLINDRICAL_SURFACE ( 'NONE', #7084, 1.499999999999999556 ) ;
#11541 = PLANE ( 'NONE',  #3282 ) ;
#11542 = CARTESIAN_POINT ( 'NONE',  ( -30.40408068685511367, 34.08504365610654219, 2.058398070974400529 ) ) ;
#11543 = ORIENTED_EDGE ( 'NONE', *, *, #6770, .F. ) ;
#11544 = CARTESIAN_POINT ( 'NONE',  ( -77.37500000204838102, 65.69163855873949842, 25.81189881250000084 ) ) ;
#11545 = VECTOR ( 'NONE', #5759, 1000.000000000000000 ) ;
#11546 = CARTESIAN_POINT ( 'NONE',  ( 47.00000000000000000, 55.00000000000000000, 0.000000000000000000 ) ) ;
#11547 = EDGE_CURVE ( 'NONE', #2344, #4746, #10563, .T. ) ;
#11548 = CARTESIAN_POINT ( 'NONE',  ( -80.00000000000000000, 55.00000000000000000, 0.000000000000000000 ) ) ;
#11549 = CARTESIAN_POINT ( 'NONE',  ( -36.85572911278101316, 38.22258139949027367, -12.89445763391127464 ) ) ;
#11550 = CARTESIAN_POINT ( 'NONE',  ( 4.999999999999998224, -2.886751345948137981, -0.4465819873852071575 ) ) ;
#11551 = CARTESIAN_POINT ( 'NONE',  ( -76.34375000204839523, 73.25176868561975141, -18.25176868561974430 ) ) ;
#11552 = DIRECTION ( 'NONE',  ( 0.000000000000000000, 0.000000000000000000, -1.000000000000000000 ) ) ;
#11553 = ORIENTED_EDGE ( 'NONE', *, *, #8805, .F. ) ;
#11554 = DIRECTION ( 'NONE',  ( 0.000000000000000000, 0.000000000000000000, 1.000000000000000000 ) ) ;
#11555 = PRODUCT_DEFINITION_CONTEXT ( 'detailed design', #1636, 'design' ) ;
#11556 = VERTEX_POINT ( 'NONE', #6035 ) ;
#11557 = CARTESIAN_POINT ( 'NONE',  ( -51.33319506590260062, 61.47761287630137161, 2.683395058215394702 ) ) ;
#11558 = DIRECTION ( 'NONE',  ( -0.000000000000000000, -0.000000000000000000, -1.000000000000000000 ) ) ;
#11559 = CARTESIAN_POINT ( 'NONE',  ( -13.54240173784083723, 59.84020960470326145, -1.295393626438009704 ) ) ;
#11560 = CARTESIAN_POINT ( 'NONE',  ( -15.00000000000000000, -30.00000000000000000, 10.00000000000000000 ) ) ;
#11561 = EDGE_CURVE ( 'NONE', #6873, #1874, #8717, .T. ) ;
#11562 = ADVANCED_FACE ( 'NONE', ( #9556 ), #6934, .F. ) ;
#11563 = CARTESIAN_POINT ( 'NONE',  ( 7.641399616170716946, 67.00208548034325418, 18.44179151512062020 ) ) ;
#11564 = CARTESIAN_POINT ( 'NONE',  ( -2.500000000000000000, 3.061616997868383141E-16, -6.099999999999999645 ) ) ;
#11565 = ORIENTED_EDGE ( 'NONE', *, *, #10157, .T. ) ;
#11566 = CARTESIAN_POINT ( 'NONE',  ( -78.21875000204839523, 29.18810118750000271, 4.741568889096522788E-15 ) ) ;
#11567 = DIRECTION ( 'NONE',  ( 0.000000000000000000, 0.000000000000000000, -1.000000000000000000 ) ) ;
#11568 = EDGE_CURVE ( 'NONE', #3028, #4578, #3203, .T. ) ;
#11569 = CIRCLE ( 'NONE', #7576, 1.500000000000001332 ) ;
#11570 = CARTESIAN_POINT ( 'NONE',  ( -80.00000000000001421, 50.75735931288069480, -14.22791868944003646 ) ) ;
#11571 = FACE_OUTER_BOUND ( 'NONE', #1634, .T. ) ;
#11572 = SURFACE_SIDE_STYLE ('',( #2542 ) ) ;
#11573 = DIRECTION ( 'NONE',  ( -1.000000000000000000, 0.000000000000000000, 0.000000000000000000 ) ) ;
#11574 = ADVANCED_FACE ( 'NONE', ( #676 ), #7761, .F. ) ;
#11575 = ORIENTED_EDGE ( 'NONE', *, *, #1685, .T. ) ;
#11576 = CARTESIAN_POINT ( 'NONE',  ( -28.29255007849803860, 50.25485254516154043, 1.609630709827212236 ) ) ;
#11577 = CARTESIAN_POINT ( 'NONE',  ( -57.50627882723209439, 66.73110044028416610, 17.54296274220338958 ) ) ;
#11578 = ORIENTED_EDGE ( 'NONE', *, *, #1308, .T. ) ;
#11579 = CARTESIAN_POINT ( 'NONE',  ( -55.66294609945612137, 69.86598917288522159, 14.86507401989504373 ) ) ;
#11580 = CARTESIAN_POINT ( 'NONE',  ( -6.496911930288724157, 57.74752198855276930, -13.79222801868778703 ) ) ;
#11581 = CARTESIAN_POINT ( 'NONE',  ( -77.56250000204838102, 80.81189881250001861, 10.69163855873948599 ) ) ;
#11582 = CIRCLE ( 'NONE', #7208, 1.500000000000001332 ) ;
#11583 = ORIENTED_EDGE ( 'NONE', *, *, #453, .T. ) ;
#11584 = CARTESIAN_POINT ( 'NONE',  ( -73.43750000000000000, 72.67766952966368876, 17.67766952966368521 ) ) ;
#11585 = CARTESIAN_POINT ( 'NONE',  ( 3.000000000000000000, 3.673940397442059868E-16, -2.617914285714285416 ) ) ;
#11586 = CARTESIAN_POINT ( 'NONE',  ( -80.00000000000001421, 71.97056274847716395, 3.371917795327861178E-06 ) ) ;
#11587 = VECTOR ( 'NONE', #10499, 1000.000000000000000 ) ;
#11588 = DIRECTION ( 'NONE',  ( -1.000000000000000000, -0.000000000000000000, -0.000000000000000000 ) ) ;
#11589 = CARTESIAN_POINT ( 'NONE',  ( -32.79192076745651008, 48.07125197820906237, 1.028503333593271174 ) ) ;
#11590 = ORIENTED_EDGE ( 'NONE', *, *, #1610, .T. ) ;
#11591 = CARTESIAN_POINT ( 'NONE',  ( 1.608176249509176925, 38.70641480386327515, -13.38147628996001792 ) ) ;
#11592 = AXIS2_PLACEMENT_3D ( 'NONE', #8442, #7367, #3886 ) ;
#11593 = CARTESIAN_POINT ( 'NONE',  ( -20.00000000000003197, -57.00000000000000000, -5.000000000000000000 ) ) ;
#11594 = CARTESIAN_POINT ( 'NONE',  ( 0.000000000000000000, 0.000000000000000000, -5.210428571428570521 ) ) ;
#11595 = CARTESIAN_POINT ( 'NONE',  ( -2.500000000000005773, -4.330127018922191873, 0.000000000000000000 ) ) ;
#11596 = CARTESIAN_POINT ( 'NONE',  ( -72.96875000204838102, 80.81189881250000440, -1.580522963032174394E-15 ) ) ;
#11597 = SHAPE_REPRESENTATION ( 'Internal Tapered Feed Screw Auger', ( #4738 ), #7754 ) ;
#11598 = EDGE_LOOP ( 'NONE', ( #5312, #6196, #8342, #9005 ) ) ;
#11599 = CARTESIAN_POINT ( 'NONE',  ( -70.93935441986300816, 80.00000000000001421, 6.698726263377743351 ) ) ;
#11600 = CARTESIAN_POINT ( 'NONE',  ( 0.000000000000000000, -17.00000000000000000, -4.171999999999999709 ) ) ;
#11601 = CARTESIAN_POINT ( 'NONE',  ( -80.00000000000001421, 67.72792206135787296, -5.742637315201482906 ) ) ;
#11602 = CARTESIAN_POINT ( 'NONE',  ( -8.839809468419982608, 72.54364378520992318, -11.73195350307014273 ) ) ;
#11603 = CIRCLE ( 'NONE', #3013, 1.500000000000001332 ) ;
#11604 = VERTEX_POINT ( 'NONE', #5248 ) ;
#11605 = CARTESIAN_POINT ( 'NONE',  ( -75.12500000204838102, 44.30836144126049447, -25.81189881249999019 ) ) ;
#11606 = AXIS2_PLACEMENT_3D ( 'NONE', #5398, #3708, #7205 ) ;
#11607 = CARTESIAN_POINT ( 'NONE',  ( -68.37000832029607977, 50.50915739122872594, 2.223033420437384500 ) ) ;
#11608 = EDGE_CURVE ( 'NONE', #1322, #9858, #1265, .T. ) ;
#11609 = PLANE ( 'NONE',  #2830 ) ;
#11610 = CARTESIAN_POINT ( 'NONE',  ( -46.39182477221876866, 68.38321102182860045, -16.29532114285349920 ) ) ;
#11611 = CARTESIAN_POINT ( 'NONE',  ( 2.712167343862819990, 4.207632145829745873, -6.100000000000002309 ) ) ;
#11612 = AXIS2_PLACEMENT_3D ( 'NONE', #5666, #11801, #9888 ) ;
#11613 = CARTESIAN_POINT ( 'NONE',  ( -78.31250000204838102, 29.18810118750000626, -10.69163855873949309 ) ) ;
#11614 = FACE_OUTER_BOUND ( 'NONE', #11598, .T. ) ;
#11615 = MECHANICAL_DESIGN_GEOMETRIC_PRESENTATION_REPRESENTATION (  '', ( #3589 ), #1674 ) ;
#11616 = ORIENTED_EDGE ( 'NONE', *, *, #151, .F. ) ;
#11617 = CARTESIAN_POINT ( 'NONE',  ( -78.00000000000001421, 63.48528137423857487, 1.500003371917795425 ) ) ;
#11618 = ORIENTED_EDGE ( 'NONE', *, *, #485, .F. ) ;
#11619 = CARTESIAN_POINT ( 'NONE',  ( 24.53746899439483187, 69.02463592203230291, 1.835796648199006231 ) ) ;
#11620 = FACE_OUTER_BOUND ( 'NONE', #6391, .T. ) ;
#11621 = EDGE_CURVE ( 'NONE', #1153, #546, #8180, .T. ) ;
#11622 = DIRECTION ( 'NONE',  ( -1.000000000000000000, -0.000000000000000000, -0.000000000000000000 ) ) ;
#11623 = VECTOR ( 'NONE', #10419, 1000.000000000000000 ) ;
#11624 = CARTESIAN_POINT ( 'NONE',  ( 21.66013690459276830, 76.95426865197336497, 1.464350659237193542 ) ) ;
#11625 = DIRECTION ( 'NONE',  ( -1.000000000000000000, -0.000000000000000000, -0.000000000000000000 ) ) ;
#11626 = ORIENTED_EDGE ( 'NONE', *, *, #11204, .T. ) ;
#11627 = CARTESIAN_POINT ( 'NONE',  ( -74.37500000204838102, 80.81189881250001861, 10.69163855873948599 ) ) ;
#11628 = DIRECTION ( 'NONE',  ( -1.000000000000000000, -0.000000000000000000, -0.000000000000000000 ) ) ;
#11629 = DIRECTION ( 'NONE',  ( -0.000000000000000000, -0.000000000000000000, -1.000000000000000000 ) ) ;
#11630 = CARTESIAN_POINT ( 'NONE',  ( 12.75940324669208792, 55.01967313903768542, -0.01734440949077138694 ) ) ;
#11631 = CARTESIAN_POINT ( 'NONE',  ( -75.00000000000004263, 35.59195408377532743, -16.92649842553838724 ) ) ;
#11632 = ORIENTED_EDGE ( 'NONE', *, *, #960, .F. ) ;
#11633 = CARTESIAN_POINT ( 'NONE',  ( -17.79452817730176406, 57.50745412809310864, 4.338269230264096166 ) ) ;
#11634 = EDGE_CURVE ( 'NONE', #6038, #518, #5706, .T. ) ;
#11635 = B_SPLINE_CURVE_WITH_KNOTS ( 'NONE', 1,
 ( #4885, #7757 ),
 .UNSPECIFIED., .F., .F.,
 ( 2, 2 ),
 ( 0.000000000000000000, 1.000000000000000000 ),
 .UNSPECIFIED. ) ;
#11636 = CARTESIAN_POINT ( 'NONE',  ( 3.556264818047235376, 3.720292241887087847, -0.08165819712376884421 ) ) ;
#11637 = ORIENTED_EDGE ( 'NONE', *, *, #3960, .F. ) ;
#11638 = CARTESIAN_POINT ( 'NONE',  ( -32.63602705562564665, 33.99332947357206081, -1.031628927963774034 ) ) ;
#11639 = CARTESIAN_POINT ( 'NONE',  ( -50.46043717566288933, 68.65163989201867878, -3.672846925086713288 ) ) ;
#11640 = AXIS2_PLACEMENT_3D ( 'NONE', #1720, #10634, #4428 ) ;
#11641 = VECTOR ( 'NONE', #8468, 1000.000000000000000 ) ;
#11642 = ORIENTED_EDGE ( 'NONE', *, *, #8074, .F. ) ;
#11643 = CARTESIAN_POINT ( 'NONE',  ( -72.87500000000000000, 30.00000000000000355, 4.592425496802573578E-15 ) ) ;
#11644 = CARTESIAN_POINT ( 'NONE',  ( 4.595919313165082620, 34.88938507153989832, -6.102095433906166377 ) ) ;
#11645 = EDGE_CURVE ( 'NONE', #879, #2912, #2196, .T. ) ;
#11646 = EDGE_CURVE ( 'NONE', #1618, #9349, #6813, .T. ) ;
#11647 =( BOUNDED_SURFACE ( )  B_SPLINE_SURFACE ( 1, 2, ( 
 ( #1979, #5525, #7451, #9175, #3906, #10121, #962, #8278, #53, #5594, #3722, #1019, #4681, #7514, #2040, #5648, #5714, #1139, #116, #3783, #11374, #2282, #4929, #4027, #3967, #5833, #7626, #6910, #11492, #303, #5958, #421, #4990, #4083, #8643, #8756, #4202, #7743, #11319, #3127, #5051, #1259, #9595, #2163, #3183, #8520, #7801, #11256, #3068, #3302, #3241, #9473, #2346, #10543, #7861, #6071, #538, #8585, #360, #5109, #6015, #1390, #7684, #1444, #9706, #2223, #9649, #11434, #6794, #6970, #4869, #4138, #6856, #10594, #10422, #2398, #6738, #5891, #10368, #9534, #1326, #10480, #8698, #481, #2461, #6249, #7148, #824, #9876 ),
 ( #8932, #2583, #1614, #1502, #7976, #9938, #11673, #4319, #9762, #4496, #3483, #6366, #8149, #11613, #5163, #8817, #598, #1562, #11789, #7028, #8993, #4262, #1672, #3415, #7920, #5341, #10651, #4444, #6129, #7206, #7090, #10713, #768, #8098, #11551, #2526, #711, #11734, #5280, #3355, #6192, #1735, #10771, #9825, #5227, #3596, #3534, #8875, #7262, #4382, #654, #8035, #10831, #2638, #10891, #6305, #5399, #9048, #2701, #41, #9102, #1968, #3655, #1066, #7320, #3836, #944, #7372, #4732, #6479, #883, #8320, #4668, #1126, #9220, #2993, #6604, #4611, #1788, #9993, #8450, #3709, #230, #4557, #8207, #5638, #10172, #1008, #6542 ) ),
 .UNSPECIFIED., .F., .F., .F. ) 
 B_SPLINE_SURFACE_WITH_KNOTS ( ( 2, 2 ),
 ( 3, 2, 2, 2, 2, 2, 2, 2, 2, 2, 2, 2, 2, 2, 2, 2, 2, 2, 2, 2, 2, 2, 2, 2, 2, 2, 2, 2, 2, 2, 2, 2, 2, 2, 2, 2, 2, 2, 2, 2, 2, 2, 2, 2, 3 ),
 ( 0.000000000000000000, 1.000000000000000000 ),
 ( 0.000000000000000000, 0.02083333333333333218, 0.04166666666666666435, 0.06250000000000000000, 0.08333333333333332871, 0.1041666666666666713, 0.1250000000000000000, 0.1458333333333333426, 0.1666666666666666574, 0.1875000000000000000, 0.2083333333333333426, 0.2291666666666666574, 0.2500000000000000000, 0.2708333333333333148, 0.2916666666666666852, 0.3125000000000000000, 0.3333333333333333148, 0.3541666666666666852, 0.3750000000000000000, 0.3958333333333333148, 0.4166666666666666852, 0.4375000000000000000, 0.4583333333333333148, 0.4791666666666666852, 0.5000000000000000000, 0.5208333333333333703, 0.5416666666666666297, 0.5625000000000000000, 0.5833333333333333703, 0.6041666666666666297, 0.6250000000000000000, 0.6458333333333333703, 0.6666666666666666297, 0.6875000000000000000, 0.7083333333333333703, 0.7291666666666666297, 0.7500000000000000000, 0.7708333333333333703, 0.7916666666666666297, 0.8125000000000000000, 0.8333333333333333703, 0.8541666666666666297, 0.8750000000000000000, 0.8888490471511721891, 0.8977375376226839343 ),
 .UNSPECIFIED. ) 
 GEOMETRIC_REPRESENTATION_ITEM ( )  RATIONAL_B_SPLINE_SURFACE ( (
 ( 1.000000000000000000, 0.9238795325112867385, 1.000000000000000000, 0.9238795325112867385, 1.000000000000000000, 0.9238795325112867385, 1.000000000000000000, 0.9238795325112867385, 1.000000000000000000, 0.9238795325112867385, 1.000000000000000000, 0.9238795325112867385, 1.000000000000000000, 0.9238795325112867385, 1.000000000000000000, 0.9238795325112867385, 1.000000000000000000, 0.9238795325112867385, 1.000000000000000000, 0.9238795325112867385, 1.000000000000000000, 0.9238795325112867385, 1.000000000000000000, 0.9238795325112867385, 1.000000000000000000, 0.9238795325112867385, 1.000000000000000000, 0.9238795325112867385, 1.000000000000000000, 0.9238795325112867385, 1.000000000000000000, 0.9238795325112867385, 1.000000000000000000, 0.9238795325112867385, 1.000000000000000000, 0.9238795325112867385, 1.000000000000000000, 0.9238795325112867385, 1.000000000000000000, 0.9238795325112867385, 1.000000000000000000, 0.9238795325112867385, 1.000000000000000000, 0.9238795325112867385, 1.000000000000000000, 0.9238795325112867385, 1.000000000000000000, 0.9238795325112867385, 1.000000000000000000, 0.9238795325112867385, 1.000000000000000000, 0.9238795325112867385, 1.000000000000000000, 0.9238795325112867385, 1.000000000000000000, 0.9238795325112867385, 1.000000000000000000, 0.9238795325112867385, 1.000000000000000000, 0.9238795325112867385, 1.000000000000000000, 0.9238795325112867385, 1.000000000000000000, 0.9238795325112867385, 1.000000000000000000, 0.9238795325112867385, 1.000000000000000000, 0.9238795325112867385, 1.000000000000000000, 0.9238795325112867385, 1.000000000000000000, 0.9238795325112867385, 1.000000000000000000, 0.9238795325112867385, 1.000000000000000000, 0.9238795325112867385, 1.000000000000000000, 0.9238795325112867385, 1.000000000000000000, 0.9238795325112867385, 1.000000000000000000, 0.9238795325112867385, 1.000000000000000000, 0.9238795325112867385, 1.000000000000000000, 0.9493985947158180005, 0.9660721892104719988, 0.9660721892104719988, 0.9660721892104719988),
 ( 1.000000000000000000, 0.9238795325112867385, 1.000000000000000000, 0.9238795325112867385, 1.000000000000000000, 0.9238795325112867385, 1.000000000000000000, 0.9238795325112867385, 1.000000000000000000, 0.9238795325112867385, 1.000000000000000000, 0.9238795325112867385, 1.000000000000000000, 0.9238795325112867385, 1.000000000000000000, 0.9238795325112867385, 1.000000000000000000, 0.9238795325112867385, 1.000000000000000000, 0.9238795325112867385, 1.000000000000000000, 0.9238795325112867385, 1.000000000000000000, 0.9238795325112867385, 1.000000000000000000, 0.9238795325112867385, 1.000000000000000000, 0.9238795325112867385, 1.000000000000000000, 0.9238795325112867385, 1.000000000000000000, 0.9238795325112867385, 1.000000000000000000, 0.9238795325112867385, 1.000000000000000000, 0.9238795325112867385, 1.000000000000000000, 0.9238795325112867385, 1.000000000000000000, 0.9238795325112867385, 1.000000000000000000, 0.9238795325112867385, 1.000000000000000000, 0.9238795325112867385, 1.000000000000000000, 0.9238795325112867385, 1.000000000000000000, 0.9238795325112867385, 1.000000000000000000, 0.9238795325112867385, 1.000000000000000000, 0.9238795325112867385, 1.000000000000000000, 0.9238795325112867385, 1.000000000000000000, 0.9238795325112867385, 1.000000000000000000, 0.9238795325112867385, 1.000000000000000000, 0.9238795325112867385, 1.000000000000000000, 0.9238795325112867385, 1.000000000000000000, 0.9238795325112867385, 1.000000000000000000, 0.9238795325112867385, 1.000000000000000000, 0.9238795325112867385, 1.000000000000000000, 0.9238795325112867385, 1.000000000000000000, 0.9238795325112867385, 1.000000000000000000, 0.9238795325112867385, 1.000000000000000000, 0.9238795325112867385, 1.000000000000000000, 0.9238795325112867385, 1.000000000000000000, 0.9238795325112867385, 1.000000000000000000, 0.9238795325112867385, 1.000000000000000000, 0.9238795325112867385, 1.000000000000000000, 0.9493985947158180005, 0.9660721892104719988, 0.9660721892104719988, 0.9660721892104719988) ) ) 
 REPRESENTATION_ITEM ( '' )  SURFACE ( )  );
#11648 = EDGE_LOOP ( 'NONE', ( #5590, #2930, #9114, #8894 ) ) ;
#11649 = DIRECTION ( 'NONE',  ( -1.000000000000000000, -0.000000000000000000, -0.000000000000000000 ) ) ;
#11650 = AXIS2_PLACEMENT_3D ( 'NONE', #10889, #3594, #8318 ) ;
#11651 = CARTESIAN_POINT ( 'NONE',  ( -79.81250000000004263, 72.67766952966367455, -17.67766952966367100 ) ) ;
#11652 = CARTESIAN_POINT ( 'NONE',  ( 3.618939467528528020, 55.00553246306094479, 0.0003573287855505533355 ) ) ;
#11653 = AXIS2_PLACEMENT_3D ( 'NONE', #825, #4497, #1907 ) ;
#11654 = VERTEX_POINT ( 'NONE', #5188 ) ;
#11655 = CARTESIAN_POINT ( 'NONE',  ( 23.52085514044975412, 76.02215512729939917, 2.750727249632518578 ) ) ;
#11656 = CARTESIAN_POINT ( 'NONE',  ( -9.969360172258976860, 70.58303384883494402, -14.12411716821732277 ) ) ;
#11657 = CARTESIAN_POINT ( 'NONE',  ( 5.000000000000000000, 2.886751345948124214, -6.099999999999999645 ) ) ;
#11658 = DIRECTION ( 'NONE',  ( 0.000000000000000000, 0.000000000000000000, 1.000000000000000000 ) ) ;
#11659 = CARTESIAN_POINT ( 'NONE',  ( -75.78125000204839523, 73.25176868561975141, 18.25176868561974075 ) ) ;
#11660 = EDGE_LOOP ( 'NONE', ( #8797, #7287, #8902, #2923 ) ) ;
#11661 = CARTESIAN_POINT ( 'NONE',  ( -73.34375000409679046, 30.00000000000001421, 10.35533905932739174 ) ) ;
#11662 = CARTESIAN_POINT ( 'NONE',  ( 0.000000000000000000, 0.000000000000000000, -25.03750572909317285 ) ) ;
#11663 = PLANE ( 'NONE',  #5020 ) ;
#11664 = VECTOR ( 'NONE', #1891, 1000.000000000000000 ) ;
#11665 = CARTESIAN_POINT ( 'NONE',  ( -34.85572910849313644, 38.22605186251247744, -12.89098713163435228 ) ) ;
#11666 = ORIENTED_EDGE ( 'NONE', *, *, #8514, .T. ) ;
#11667 = FACE_OUTER_BOUND ( 'NONE', #740, .T. ) ;
#11668 = CARTESIAN_POINT ( 'NONE',  ( -78.00000000000002842, 42.27207793864211283, 2.742644059037075976 ) ) ;
#11669 = ORIENTED_EDGE ( 'NONE', *, *, #7349, .F. ) ;
#11670 = DIRECTION ( 'NONE',  ( -1.000000000000000000, 0.000000000000000000, 0.000000000000000000 ) ) ;
#11671 = CIRCLE ( 'NONE', #11477, 5.000000000000000888 ) ;
#11672 = CARTESIAN_POINT ( 'NONE',  ( 18.34332550980965593, 58.97478973010875336, 3.050963776907112290 ) ) ;
#11673 = CARTESIAN_POINT ( 'NONE',  ( -78.96875000204839523, 73.25176868561975141, 18.25176868561974075 ) ) ;
#11674 = DIRECTION ( 'NONE',  ( -1.000000000000000000, 0.000000000000000000, 0.000000000000000000 ) ) ;
#11675 = ORIENTED_EDGE ( 'NONE', *, *, #9295, .T. ) ;
#11676 = CARTESIAN_POINT ( 'NONE',  ( 2.500000000000000000, 0.000000000000000000, -6.099999999999999645 ) ) ;
#11677 = CIRCLE ( 'NONE', #2705, 5.000000000000000000 ) ;
#11678 = EDGE_LOOP ( 'NONE', ( #7266, #83, #5088, #870, #8710, #5735, #2490, #3126, #2476, #5059 ) ) ;
#11679 = CARTESIAN_POINT ( 'NONE',  ( 1.656070432594679565, 51.94480720268091289, -3.971655978929947484 ) ) ;
#11680 = CARTESIAN_POINT ( 'NONE',  ( 12.87292705410422577, 47.94148912775095539, 12.25634023971492503 ) ) ;
#11681 = AXIS2_PLACEMENT_3D ( 'NONE', #7553, #6537, #4009 ) ;
#11682 = DIRECTION ( 'NONE',  ( 0.000000000000000000, 0.000000000000000000, 1.000000000000000000 ) ) ;
#11683 = DIRECTION ( 'NONE',  ( 1.000000000000000000, -0.000000000000000000, -0.000000000000000000 ) ) ;
#11684 = CARTESIAN_POINT ( 'NONE',  ( -78.00000000000001421, 54.99999999999998579, -6.985278002320760571 ) ) ;
#11685 = CIRCLE ( 'NONE', #4808, 22.00000000000000000 ) ;
#11686 = AXIS2_PLACEMENT_3D ( 'NONE', #6850, #2520, #9817 ) ;
#11687 = CARTESIAN_POINT ( 'NONE',  ( -72.50000000204836681, 29.18810118750000981, 10.69163855873950020 ) ) ;
#11688 = ORIENTED_EDGE ( 'NONE', *, *, #11608, .T. ) ;
#11689 = EDGE_CURVE ( 'NONE', #760, #1948, #11123, .T. ) ;
#11690 = DIRECTION ( 'NONE',  ( -1.000000000000000000, -0.000000000000000000, -0.000000000000000000 ) ) ;
#11691 = CARTESIAN_POINT ( 'NONE',  ( -74.75000000204840944, 65.69163855873948421, -25.81189881250000440 ) ) ;
#11692 = DIRECTION ( 'NONE',  ( -1.000000000000000000, -0.000000000000000000, -0.000000000000000000 ) ) ;
#11693 = UNCERTAINTY_MEASURE_WITH_UNIT (LENGTH_MEASURE( 1.000000000000000082E-05 ), #10298, 'distance_accuracy_value', 'NONE');
#11694 = VECTOR ( 'NONE', #2628, 1000.000000000000000 ) ;
#11695 = EDGE_CURVE ( 'NONE', #3150, #2768, #905, .T. ) ;
#11696 = CARTESIAN_POINT ( 'NONE',  ( -76.81250000409679046, 72.67766952966368876, 17.67766952966368521 ) ) ;
#11697 = CARTESIAN_POINT ( 'NONE',  ( -12.09272392674168017, 55.02619396104714866, 0.001659151704244336443 ) ) ;
#11698 = CARTESIAN_POINT ( 'NONE',  ( 0.000000000000000000, 0.000000000000000000, 0.000000000000000000 ) ) ;
#11699 = VECTOR ( 'NONE', #5181, 1000.000000000000000 ) ;
#11700 = DIRECTION ( 'NONE',  ( -1.000000000000000000, -0.000000000000000000, -0.000000000000000000 ) ) ;
#11701 = ORIENTED_EDGE ( 'NONE', *, *, #3917, .T. ) ;
#11702 = CARTESIAN_POINT ( 'NONE',  ( -80.00000000000002842, 42.27207793864211283, 12.72792543327562775 ) ) ;
#11703 = CARTESIAN_POINT ( 'NONE',  ( 5.000000000000000000, 2.886751345948134428, -0.4465819873852071575 ) ) ;
#11704 = ORIENTED_EDGE ( 'NONE', *, *, #1610, .F. ) ;
#11705 = CARTESIAN_POINT ( 'NONE',  ( -42.54809234475217039, 58.08538739954438057, -20.80116627830041054 ) ) ;
#11706 = CARTESIAN_POINT ( 'NONE',  ( -78.12500000204838102, 44.30836144126050158, -25.81189881249999374 ) ) ;
#11707 = EDGE_LOOP ( 'NONE', ( #10158, #3639, #8411, #10511 ) ) ;
#11708 = CARTESIAN_POINT ( 'NONE',  ( -76.53125000204838102, 55.00000000000000000, -25.81189881249999729 ) ) ;
#11709 = CARTESIAN_POINT ( 'NONE',  ( 18.81101721030213625, 65.56418867429738384, 18.32872549916029925 ) ) ;
#11710 = ORIENTED_EDGE ( 'NONE', *, *, #9539, .F. ) ;
#11711 = CARTESIAN_POINT ( 'NONE',  ( -79.53125000204838102, 55.00000000000000000, -25.81189881249999729 ) ) ;
#11712 = CARTESIAN_POINT ( 'NONE',  ( 15.64624132220377639, 54.34386165159118320, 4.967374051144239466 ) ) ;
#11713 = CARTESIAN_POINT ( 'NONE',  ( -69.44401486253393330, 48.16327053899182431, 1.838581984797913460 ) ) ;
#11714 = ORIENTED_EDGE ( 'NONE', *, *, #11056, .F. ) ;
#11715 = CARTESIAN_POINT ( 'NONE',  ( -62.51030605291772702, 43.28161195024001273, 17.55542603392786916 ) ) ;
#11716 = CARTESIAN_POINT ( 'NONE',  ( -28.94161417925737823, 38.68453375511723635, 13.40299329694203578 ) ) ;
#11717 = PLANE ( 'NONE',  #8693 ) ;
#11718 = EDGE_CURVE ( 'NONE', #8495, #1970, #3781, .T. ) ;
#11719 = CARTESIAN_POINT ( 'NONE',  ( -80.00000000000002842, 46.51471862576140381, 6.985284746156355418 ) ) ;
#11720 = DIRECTION ( 'NONE',  ( 0.000000000000000000, 0.000000000000000000, 1.000000000000000000 ) ) ;
#11721 = ORIENTED_EDGE ( 'NONE', *, *, #9063, .T. ) ;
#11722 =( BOUNDED_CURVE ( )  B_SPLINE_CURVE ( 2, ( #4920, #2270, #5826, #8746, #5945, #3058, #8572, #4192, #529 ),
 .UNSPECIFIED., .F., .T. ) 
 B_SPLINE_CURVE_WITH_KNOTS ( ( 3, 2, 2, 2, 3 ),
 ( 0.3960654071566668821, 0.4158759072859810613, 0.4356864074152952404, 0.4554969075446094751, 0.4753074076739236542 ),
 .UNSPECIFIED. ) 
 CURVE ( )  GEOMETRIC_REPRESENTATION_ITEM ( )  RATIONAL_B_SPLINE_CURVE ( ( 1.000000000000000000, 0.9238795325112867385, 1.000000000000000000, 0.9238795325112867385, 1.000000000000000000, 0.9238795325112867385, 1.000000000000000000, 0.9238795325111756052, 1.000000000000111244 ) ) 
 REPRESENTATION_ITEM ( '' )  );
#11723 = CARTESIAN_POINT ( 'NONE',  ( 36.99999999999999289, 59.99999999999998579, 0.000000000000000000 ) ) ;
#11724 = PLANE ( 'NONE',  #8796 ) ;
#11725 = DIRECTION ( 'NONE',  ( -1.000000000000000000, 0.000000000000000000, 0.000000000000000000 ) ) ;
#11726 = CARTESIAN_POINT ( 'NONE',  ( -50.27495406422890767, 76.01781437481966464, 2.059423474151367728 ) ) ;
#11727 = ORIENTED_EDGE ( 'NONE', *, *, #11547, .T. ) ;
#11728 = DIRECTION ( 'NONE',  ( 1.000000000000000000, 0.000000000000000000, 0.000000000000000000 ) ) ;
#11729 = ADVANCED_FACE ( 'NONE', ( #5305 ), #331, .F. ) ;
#11730 = DIRECTION ( 'NONE',  ( 0.000000000000000000, -0.000000000000000000, 1.000000000000000000 ) ) ;
#11731 = ORIENTED_EDGE ( 'NONE', *, *, #6841, .F. ) ;
#11732 = CARTESIAN_POINT ( 'NONE',  ( -78.00000000000001421, 59.24264068711927678, 2.742644059037073312 ) ) ;
#11733 = DIRECTION ( 'NONE',  ( 0.000000000000000000, 0.000000000000000000, 1.000000000000000000 ) ) ;
#11734 = CARTESIAN_POINT ( 'NONE',  ( -76.06250000204839523, 80.81189881250001861, 10.69163855873948599 ) ) ;
#11735 = CARTESIAN_POINT ( 'NONE',  ( -79.25000000204838102, 80.81189881250001861, -10.69163855873949132 ) ) ;
#11736 = EDGE_LOOP ( 'NONE', ( #7362, #6784, #8100, #4015, #1078, #11710 ) ) ;
#11737 = FACE_OUTER_BOUND ( 'NONE', #1187, .T. ) ;
#11738 = ORIENTED_EDGE ( 'NONE', *, *, #3807, .F. ) ;
#11739 = CARTESIAN_POINT ( 'NONE',  ( 0.4285831363683495487, 65.42943686846955131, 22.72062601704910989 ) ) ;
#11740 = CARTESIAN_POINT ( 'NONE',  ( -24.46043788332341151, 47.94142141767103737, 12.25631317379969509 ) ) ;
#11741 = CARTESIAN_POINT ( 'NONE',  ( -78.78125000204839523, 73.25176868561975141, 18.25176868561974075 ) ) ;
#11742 = CARTESIAN_POINT ( 'NONE',  ( -77.37500000409677625, 55.00000000000000000, -24.99999999999999645 ) ) ;
#11743 = LINE ( 'NONE', #5290, #8570 ) ;
#11744 = CARTESIAN_POINT ( 'NONE',  ( -74.18750000204838102, 44.30836144126052289, 25.81189881250000795 ) ) ;
#11745 = ORIENTED_EDGE ( 'NONE', *, *, #8926, .T. ) ;
#11746 = CARTESIAN_POINT ( 'NONE',  ( -75.87500000204839523, 80.81189881250001861, 10.69163855873948599 ) ) ;
#11747 = CARTESIAN_POINT ( 'NONE',  ( -20.00000000000003197, -57.00000000000000000, -5.000000000000000000 ) ) ;
#11748 = CARTESIAN_POINT ( 'NONE',  ( 0.000000000000000000, 0.000000000000000000, -0.3851141460153411078 ) ) ;
#11749 = CARTESIAN_POINT ( 'NONE',  ( -40.20488286162279223, 55.00025610236561846, -0.004523070879801337381 ) ) ;
#11750 = DIRECTION ( 'NONE',  ( 1.000000000000000000, 0.000000000000000000, -0.000000000000000000 ) ) ;
#11751 = ORIENTED_EDGE ( 'NONE', *, *, #4225, .T. ) ;
#11752 = DIRECTION ( 'NONE',  ( 1.000000000000000000, 6.033820786006286457E-17, 0.000000000000000000 ) ) ;
#11753 = CARTESIAN_POINT ( 'NONE',  ( 2.500000000000005773, 4.330127018922190985, 0.000000000000000000 ) ) ;
#11754 = ORIENTED_EDGE ( 'NONE', *, *, #35, .T. ) ;
#11755 = EDGE_CURVE ( 'NONE', #3047, #2139, #4158, .T. ) ;
#11756 = CARTESIAN_POINT ( 'NONE',  ( -30.59602397924764361, 34.87358162761611169, 6.107823804857911654 ) ) ;
#11757 = CARTESIAN_POINT ( 'NONE',  ( -75.31250000204839523, 29.18810118750000626, -10.69163855873949309 ) ) ;
#11758 = MECHANICAL_DESIGN_GEOMETRIC_PRESENTATION_REPRESENTATION (  '', ( #11169 ), #2199 ) ;
#11759 = VECTOR ( 'NONE', #10394, 1000.000000000000000 ) ;
#11760 = ORIENTED_EDGE ( 'NONE', *, *, #10614, .T. ) ;
#11761 = CARTESIAN_POINT ( 'NONE',  ( -71.65625000204838102, 80.81189881250000440, -1.580522963032174394E-15 ) ) ;
#11762 = CARTESIAN_POINT ( 'NONE',  ( -18.45202553953894764, 65.80723110900194683, 18.02933743899848551 ) ) ;
#11763 = EDGE_CURVE ( 'NONE', #4892, #847, #2777, .T. ) ;
#11764 = LINE ( 'NONE', #5317, #10675 ) ;
#11765 = CARTESIAN_POINT ( 'NONE',  ( -2.092693678294518467, 54.98959697584933792, -0.01274811450331606207 ) ) ;
#11766 = VECTOR ( 'NONE', #2990, 1000.000000000000000 ) ;
#11767 = ORIENTED_EDGE ( 'NONE', *, *, #4700, .T. ) ;
#11768 = CARTESIAN_POINT ( 'NONE',  ( -8.329477863459651132, 69.86497200091255877, -14.86570652194256148 ) ) ;
#11769 = CARTESIAN_POINT ( 'NONE',  ( -15.85565286160008469, 75.43490621471428881, 5.492246195135631837 ) ) ;
#11770 = PRESENTATION_STYLE_ASSIGNMENT (( #9920 ) ) ;
#11771 = DIRECTION ( 'NONE',  ( 0.000000000000000000, 1.000000000000000000, 0.000000000000000000 ) ) ;
#11772 = CARTESIAN_POINT ( 'NONE',  ( -3.346878500200761053, -3.841181488860384796, -6.048595712916170264 ) ) ;
#11773 = ORIENTED_EDGE ( 'NONE', *, *, #1915, .F. ) ;
#11774 = CARTESIAN_POINT ( 'NONE',  ( -70.87427368927673399, 76.65063840437989029, 12.49999426731031704 ) ) ;
#11775 = CYLINDRICAL_SURFACE ( 'NONE', #1328, 1.499999999999999556 ) ;
#11776 = FACE_BOUND ( 'NONE', #2606, .T. ) ;
#11777 = AXIS2_PLACEMENT_3D ( 'NONE', #3321, #6988, #10611 ) ;
#11778 = ADVANCED_FACE ( 'NONE', ( #6383 ), #3502, .T. ) ;
#11779 = VERTEX_POINT ( 'NONE', #10737 ) ;
#11780 = CARTESIAN_POINT ( 'NONE',  ( 0.000000000000000000, 0.000000000000000000, -5.000000000000000000 ) ) ;
#11781 = CIRCLE ( 'NONE', #7970, 2.999999999999995559 ) ;
#11782 = CARTESIAN_POINT ( 'NONE',  ( -53.98894970602387389, 59.83948248508205836, 1.298372112287061508 ) ) ;
#11783 = ORIENTED_EDGE ( 'NONE', *, *, #1485, .F. ) ;
#11784 = DIRECTION ( 'NONE',  ( -1.000000000000000000, 0.000000000000000000, 0.000000000000000000 ) ) ;
#11785 = EDGE_CURVE ( 'NONE', #1312, #849, #4938, .T. ) ;
#11786 = CARTESIAN_POINT ( 'NONE',  ( -78.00000000000002842, 42.27207793864211283, 14.22792543327562775 ) ) ;
#11787 = EDGE_CURVE ( 'NONE', #1948, #4670, #10827, .T. ) ;
#11788 = DIRECTION ( 'NONE',  ( -1.000000000000000000, 0.000000000000000000, -0.000000000000000000 ) ) ;
#11789 = CARTESIAN_POINT ( 'NONE',  ( -77.84375000204839523, 73.25176868561975141, -18.25176868561974430 ) ) ;
#11790 = CARTESIAN_POINT ( 'NONE',  ( -78.78125000204838102, 55.00000000000000000, 25.81189881249999729 ) ) ;
#11791 = ORIENTED_EDGE ( 'NONE', *, *, #6586, .T. ) ;
#11792 = EDGE_CURVE ( 'NONE', #3881, #4551, #7326, .T. ) ;
#11793 = CIRCLE ( 'NONE', #11592, 1.500000000000001332 ) ;
#11794 = CARTESIAN_POINT ( 'NONE',  ( -74.93750000204839523, 44.30836144126050158, -25.81189881249999374 ) ) ;
#11795 = EDGE_LOOP ( 'NONE', ( #2816, #1232, #7647 ) ) ;
#11796 = CARTESIAN_POINT ( 'NONE',  ( 16.17279400537643852, 72.62292825401752339, 17.77849829575843543 ) ) ;
#11797 = AXIS2_PLACEMENT_3D ( 'NONE', #8448, #11063, #1065 ) ;
#11798 = CARTESIAN_POINT ( 'NONE',  ( -7.630320567153270339, 65.39170505435430414, -9.418633508564214551 ) ) ;
#11799 = CARTESIAN_POINT ( 'NONE',  ( -75.59375000204839523, 55.00000000000000000, 25.81189881249999729 ) ) ;
#11800 = CARTESIAN_POINT ( 'NONE',  ( -3.000000000000000888, 0.000000000000000000, -6.074599999999999334 ) ) ;
#11801 = DIRECTION ( 'NONE',  ( -1.000000000000000000, -0.000000000000000000, -0.000000000000000000 ) ) ;
#11802 = AXIS2_PLACEMENT_3D ( 'NONE', #2258, #2202, #5814 ) ;
#11803 =( GEOMETRIC_REPRESENTATION_CONTEXT ( 3 ) GLOBAL_UNCERTAINTY_ASSIGNED_CONTEXT ( ( #4400 ) ) GLOBAL_UNIT_ASSIGNED_CONTEXT ( ( #4417, #5373, #7124 ) ) REPRESENTATION_CONTEXT ( 'NONE', 'WORKASPACE' ) );
#11804 = EDGE_LOOP ( 'NONE', ( #2427, #4488, #3254, #5152, #2221, #10628 ) ) ;
#11805 = CARTESIAN_POINT ( 'NONE',  ( -76.25000000409677625, 30.00000000000000355, 4.592425496802573578E-15 ) ) ;
#11806 = CARTESIAN_POINT ( 'NONE',  ( -75.31250000409677625, 72.67766952966368876, 17.67766952966368521 ) ) ;
#11807 = DIRECTION ( 'NONE',  ( -1.000000000000000000, -0.000000000000000000, -0.000000000000000000 ) ) ;
#11808 = DIRECTION ( 'NONE',  ( -1.000000000000000000, 0.000000000000000000, 0.000000000000000000 ) ) ;
#11809 = CARTESIAN_POINT ( 'NONE',  ( -59.75812396593624243, 55.00560539528500215, -0.01061549039029876899 ) ) ;
#11810 = CIRCLE ( 'NONE', #8188, 2.500000000000000000 ) ;
#11811 = CARTESIAN_POINT ( 'NONE',  ( -21.50191578866859388, 76.82143766378479199, 2.891252975302713857 ) ) ;
#11812 = CARTESIAN_POINT ( 'NONE',  ( -18.95867291721290471, 56.61031706631060700, 4.744919608251485954 ) ) ;
#11813 = ORIENTED_EDGE ( 'NONE', *, *, #726, .F. ) ;
#11814 = CARTESIAN_POINT ( 'NONE',  ( 3.346878500200757056, 3.841181488860378135, -0.05140428708382578649 ) ) ;
#11815 = ORIENTED_EDGE ( 'NONE', *, *, #7328, .F. ) ;
#11816 = CARTESIAN_POINT ( 'NONE',  ( -7.337209909475700620, 63.04728967918421745, -19.42673836724018699 ) ) ;
#11817 = CARTESIAN_POINT ( 'NONE',  ( -77.46875000204839523, 80.81189881250000440, -1.580522963032174394E-15 ) ) ;
#11818 = ORIENTED_EDGE ( 'NONE', *, *, #5965, .T. ) ;
#11819 = CARTESIAN_POINT ( 'NONE',  ( -73.90625000204838102, 29.18810118750000271, 4.741568889096522788E-15 ) ) ;
#11820 = CARTESIAN_POINT ( 'NONE',  ( -30.40408068685511367, 34.08504365610654219, 2.058398070974400529 ) ) ;
#11821 = EDGE_CURVE ( 'NONE', #7813, #8716, #5719, .T. ) ;
#11822 = VERTEX_POINT ( 'NONE', #6549 ) ;
#11823 = CARTESIAN_POINT ( 'NONE',  ( -79.34375000204839523, 55.00000000000000000, -25.81189881249999729 ) ) ;
#11824 = CARTESIAN_POINT ( 'NONE',  ( -62.24957892231395817, 54.31321652181242854, 6.980810767642831927 ) ) ;
#11825 = ORIENTED_EDGE ( 'NONE', *, *, #55, .T. ) ;
#11826 = CARTESIAN_POINT ( 'NONE',  ( 22.81087673974644403, 75.43171151743705138, 5.491419164873361680 ) ) ;
#11827 = CARTESIAN_POINT ( 'NONE',  ( -21.32947787934852357, 63.04568470447853912, 19.42265540296757464 ) ) ;
#11828 = CARTESIAN_POINT ( 'NONE',  ( 5.000000000000000000, -0.4878135028931874784, 5.353248226647178143E-16 ) ) ;
#11829 = DIRECTION ( 'NONE',  ( 0.000000000000000000, 0.000000000000000000, -1.000000000000000000 ) ) ;
#11830 = DIRECTION ( 'NONE',  ( -0.000000000000000000, -1.000000000000000000, -0.000000000000000000 ) ) ;
#11831 = EDGE_LOOP ( 'NONE', ( #1963, #11637, #1531, #6735 ) ) ;
#11832 = CARTESIAN_POINT ( 'NONE',  ( 0.000000000000000000, 0.000000000000000000, -2.617914285714285416 ) ) ;
#11833 = CARTESIAN_POINT ( 'NONE',  ( -47.43046783121353371, 54.99045398927809458, 0.007802215875459363355 ) ) ;
#11834 = CARTESIAN_POINT ( 'NONE',  ( -55.71338727784861788, 57.06385637567746727, 4.557138327899026287 ) ) ;
#11835 = VECTOR ( 'NONE', #9146, 1000.000000000000000 ) ;
#11836 = DIRECTION ( 'NONE',  ( 0.000000000000000000, 1.000000000000000000, 0.000000000000000000 ) ) ;
#11837 = CIRCLE ( 'NONE', #10113, 1.500000000000001332 ) ;
#11838 = CARTESIAN_POINT ( 'NONE',  ( -74.65625000409679046, 30.00000000000000355, -10.35533905932738108 ) ) ;
#11839 = VERTEX_POINT ( 'NONE', #11247 ) ;
#11840 = DIRECTION ( 'NONE',  ( -1.000000000000000000, 0.000000000000000000, -0.000000000000000000 ) ) ;
#11841 = CARTESIAN_POINT ( 'NONE',  ( 0.000000000000000000, 0.000000000000000000, -6.099999999999999645 ) ) ;
#11842 = CARTESIAN_POINT ( 'NONE',  ( 14.45936532742768321, 56.29682532305226772, 4.839835512798248196 ) ) ;
#11843 = DIRECTION ( 'NONE',  ( -1.000000000000000000, -0.000000000000000000, -0.000000000000000000 ) ) ;
#11844 = CARTESIAN_POINT ( 'NONE',  ( -76.53125000204838102, 55.00000000000000000, -25.81189881249999729 ) ) ;
#11845 = AXIS2_PLACEMENT_3D ( 'NONE', #8466, #3850, #2951 ) ;
#11846 = ORIENTED_EDGE ( 'NONE', *, *, #8290, .F. ) ;
#11847 = CARTESIAN_POINT ( 'NONE',  ( -74.56250000204839523, 80.81189881250001861, -10.69163855873949132 ) ) ;
#11848 = ORIENTED_EDGE ( 'NONE', *, *, #4153, .T. ) ;
#11849 = CARTESIAN_POINT ( 'NONE',  ( 0.8701179677062256257, 52.49160040349491396, -4.337762753772214985 ) ) ;
#11850 = CARTESIAN_POINT ( 'NONE',  ( -3.830245506239644548, 57.74702083132989117, -13.79104772941276025 ) ) ;
#11851 = ADVANCED_FACE ( 'NONE', ( #3059 ), #11070, .F. ) ;
#11852 = CARTESIAN_POINT ( 'NONE',  ( 34.00000000000000000, 45.00000000000001421, 1.224646799147351679E-15 ) ) ;
#11853 = EDGE_CURVE ( 'NONE', #1798, #10795, #7429, .T. ) ;
#11854 = NEXT_ASSEMBLY_USAGE_OCCURRENCE ( 'NAUO1', ' ', ' ', #9810, #133, $ ) ;
#11855 = NEXT_ASSEMBLY_USAGE_OCCURRENCE ( 'NAUO2', ' ', ' ', #9810, #3148, $ ) ;
#11856 = NEXT_ASSEMBLY_USAGE_OCCURRENCE ( 'NAUO3', ' ', ' ', #9810, #1895, $ ) ;
#11857 = NEXT_ASSEMBLY_USAGE_OCCURRENCE ( 'NAUO4', ' ', ' ', #9810, #4545, $ ) ;
#11858 = NEXT_ASSEMBLY_USAGE_OCCURRENCE ( 'NAUO5', ' ', ' ', #9810, #4032, $ ) ;
#11859 = NEXT_ASSEMBLY_USAGE_OCCURRENCE ( 'NAUO6', ' ', ' ', #9810, #2197, $ ) ;
#11860 = NEXT_ASSEMBLY_USAGE_OCCURRENCE ( 'NAUO7', ' ', ' ', #9810, #3298, $ ) ;
#11861=COLOUR_RGB('Dark Blue',0.08,0.2,0.34);
#11862=FILL_AREA_STYLE_COLOUR('',#11861);
#11863=FILL_AREA_STYLE('',(#11862));
#11864=SURFACE_STYLE_FILL_AREA(#11863);
#11865=SURFACE_SIDE_STYLE('',(#11864));
#11866=SURFACE_STYLE_USAGE(.BOTH.,#11865);
#11867=PRESENTATION_STYLE_ASSIGNMENT((#11866));
#11868=COLOUR_RGB('Light Blue',0.38,0.62,0.78);
#11869=FILL_AREA_STYLE_COLOUR('',#11868);
#11870=FILL_AREA_STYLE('',(#11869));
#11871=SURFACE_STYLE_FILL_AREA(#11870);
#11872=SURFACE_SIDE_STYLE('',(#11871));
#11873=SURFACE_STYLE_USAGE(.BOTH.,#11872);
#11874=PRESENTATION_STYLE_ASSIGNMENT((#11873));
#11875=COLOUR_RGB('Sky Blue',0.24,0.69,0.87);
#11876=FILL_AREA_STYLE_COLOUR('',#11875);
#11877=FILL_AREA_STYLE('',(#11876));
#11878=SURFACE_STYLE_FILL_AREA(#11877);
#11879=SURFACE_SIDE_STYLE('',(#11878));
#11880=SURFACE_STYLE_USAGE(.BOTH.,#11879);
#11881=PRESENTATION_STYLE_ASSIGNMENT((#11880));
#11882=COLOUR_RGB('Grey',0.48,0.52,0.57);
#11883=FILL_AREA_STYLE_COLOUR('',#11882);
#11884=FILL_AREA_STYLE('',(#11883));
#11885=SURFACE_STYLE_FILL_AREA(#11884);
#11886=SURFACE_SIDE_STYLE('',(#11885));
#11887=SURFACE_STYLE_USAGE(.BOTH.,#11886);
#11888=PRESENTATION_STYLE_ASSIGNMENT((#11887));
#11889=COLOUR_RGB('Black',0.12,0.14,0.17);
#11890=FILL_AREA_STYLE_COLOUR('',#11889);
#11891=FILL_AREA_STYLE('',(#11890));
#11892=SURFACE_STYLE_FILL_AREA(#11891);
#11893=SURFACE_SIDE_STYLE('',(#11892));
#11894=SURFACE_STYLE_USAGE(.BOTH.,#11893);
#11895=PRESENTATION_STYLE_ASSIGNMENT((#11894));
#11896=COLOUR_RGB('Off White',0.89,0.88,0.83);
#11897=FILL_AREA_STYLE_COLOUR('',#11896);
#11898=FILL_AREA_STYLE('',(#11897));
#11899=SURFACE_STYLE_FILL_AREA(#11898);
#11900=SURFACE_SIDE_STYLE('',(#11899));
#11901=SURFACE_STYLE_USAGE(.BOTH.,#11900);
#11902=PRESENTATION_STYLE_ASSIGNMENT((#11901));
ENDSEC;
END-ISO-10303-21;
